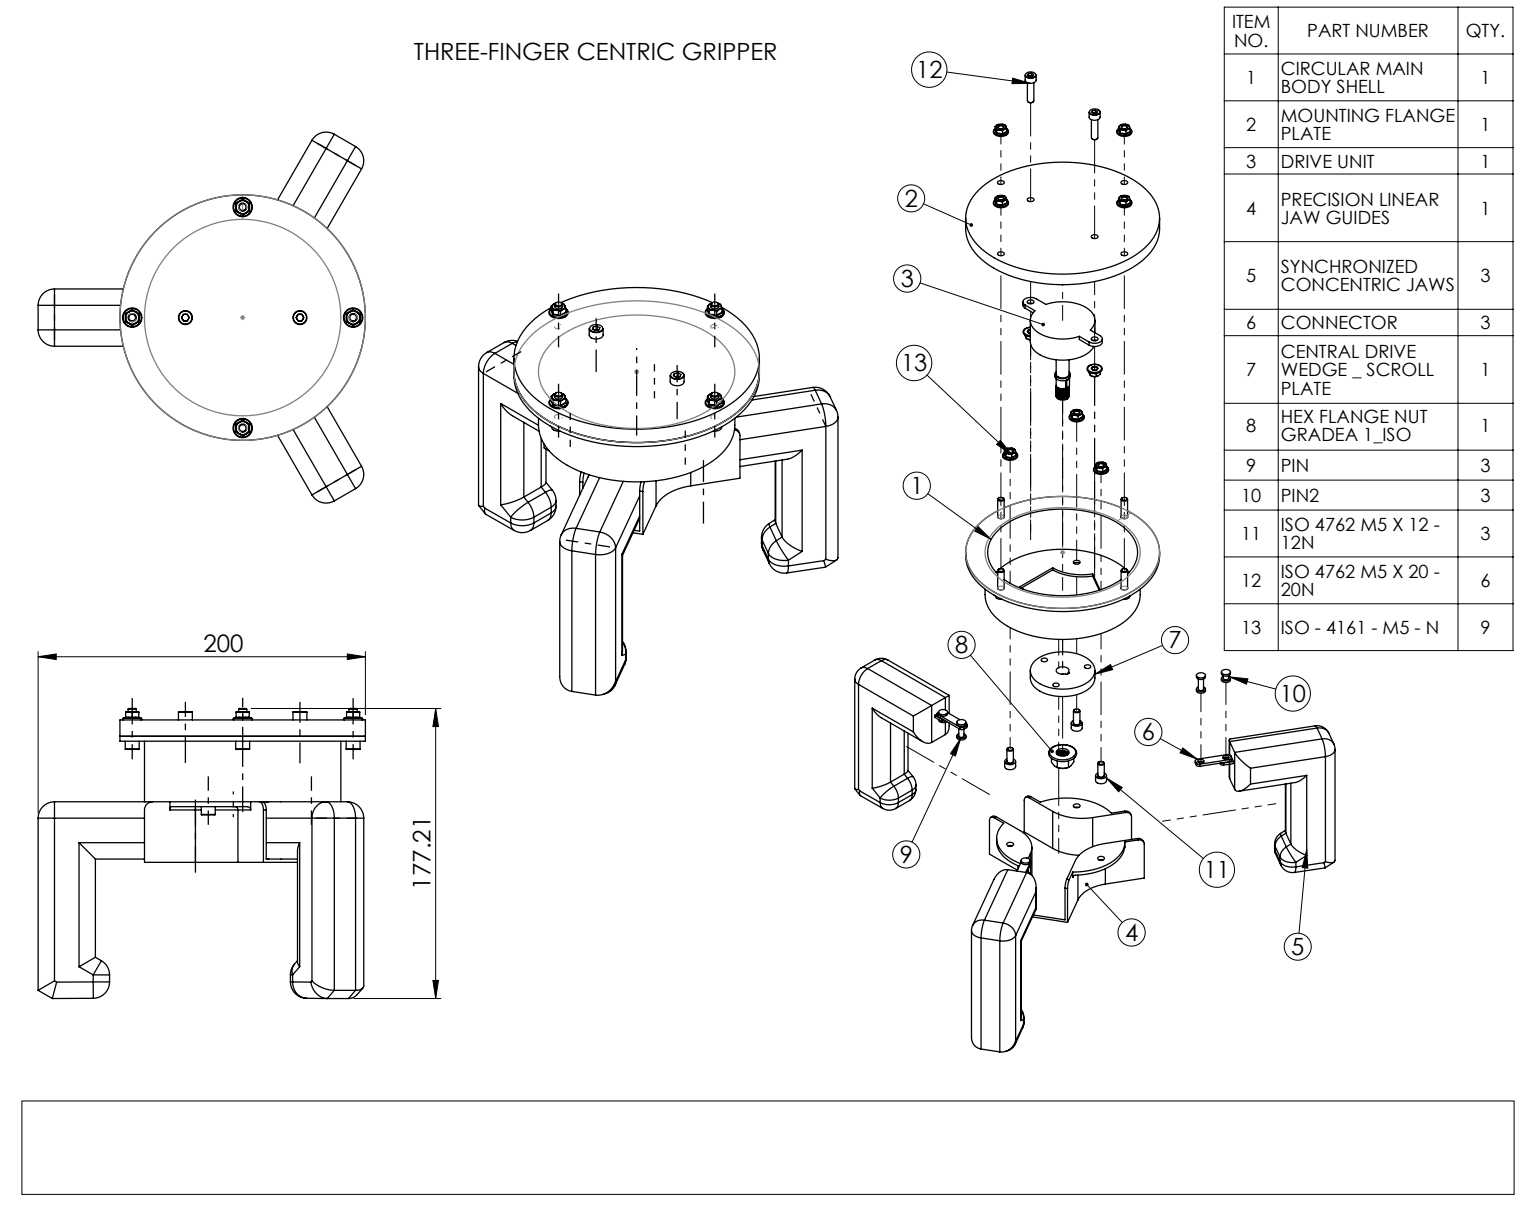
ISO-10303-21;
HEADER;
FILE_DESCRIPTION (('STEP AP214'),
    '1' );
FILE_NAME ('BR-003',
    '2026-10-08T13:56:24',
    ( '' ),
    ( '' ),
    'SwSTEP 2.0',
    'SolidWorks 2026',
    '' );
FILE_SCHEMA (( 'AUTOMOTIVE_DESIGN' ));
ENDSEC;

DATA;
#1 = ORIENTED_EDGE ( 'NONE', *, *, #6878, .F. ) ;
#2 = EDGE_CURVE ( 'NONE', #5376, #11920, #8952, .T. ) ;
#3 = CARTESIAN_POINT ( 'NONE',  ( -7.500000000000003553, -3.160302461882598557, -7.231849989190477501 ) ) ;
#4 = CARTESIAN_POINT ( 'NONE',  ( -1.846868145590737420, -24.75000000136559564, 4.458734124999999437 ) ) ;
#5 = FACE_OUTER_BOUND ( 'NONE', #2226, .T. ) ;
#6 = VERTEX_POINT ( 'NONE', #1075 ) ;
#7 = CARTESIAN_POINT ( 'NONE',  ( -19.99999999999956657, -20.00000000000000000, 2.500000000000877520 ) ) ;
#8 = CARTESIAN_POINT ( 'NONE',  ( 0.000000000000000000, 50.00000000000000000, -75.00000000000004263 ) ) ;
#9 = DIRECTION ( 'NONE',  ( -1.000000000000000000, -0.000000000000000000, -0.000000000000000000 ) ) ;
#10 = FACE_OUTER_BOUND ( 'NONE', #8516, .T. ) ;
#11 = CARTESIAN_POINT ( 'NONE',  ( 1.846868145590735200, -25.50000000136559919, -4.458734125000000326 ) ) ;
#12 = DIRECTION ( 'NONE',  ( 0.000000000000000000, 0.000000000000000000, 1.000000000000000000 ) ) ;
#13 =( REPRESENTATION_RELATIONSHIP ('NONE','NONE', #4176, #790 ) REPRESENTATION_RELATIONSHIP_WITH_TRANSFORMATION ( #11413 )SHAPE_REPRESENTATION_RELATIONSHIP( ) );
#14 = CARTESIAN_POINT ( 'NONE',  ( 19.99999999999956657, -8.786575603324269439E-13, 0.000000000000000000 ) ) ;
#15 = CARTESIAN_POINT ( 'NONE',  ( -3.535533905932738641, -28.50000000273118772, 3.535533905932737309 ) ) ;
#16 = CARTESIAN_POINT ( 'NONE',  ( 7.922281120364393914, 4.573931137438269623, -8.047472243342932430 ) ) ;
#17 = CARTESIAN_POINT ( 'NONE',  ( 3.152801135295367541, -29.31250000136559208, -3.152801135295367541 ) ) ;
#18 = ADVANCED_FACE ( 'NONE', ( #40 ), #4954, .F. ) ;
#19 = CYLINDRICAL_SURFACE ( 'NONE', #13536, 2.649999999999992806 ) ;
#21 = ADVANCED_FACE ( 'NONE', ( #13423 ), #15876, .F. ) ;
#20 = ORIENTED_EDGE ( 'NONE', *, *, #13802, .F. ) ;
#22 = EDGE_CURVE ( 'NONE', #14589, #7997, #9723, .T. ) ;
#23 = SURFACE_STYLE_FILL_AREA ( #9793 ) ;
#24 = ORIENTED_EDGE ( 'NONE', *, *, #9310, .F. ) ;
#25 = DIRECTION ( 'NONE',  ( -0.000000000000000000, -1.000000000000000000, -0.000000000000000000 ) ) ;
#26 = ORIENTED_EDGE ( 'NONE', *, *, #11739, .T. ) ;
#27 = FACE_BOUND ( 'NONE', #8966, .T. ) ;
#28 = CARTESIAN_POINT ( 'NONE',  ( 2.500000000000000000, -1.768423874527823569, 1.021000000000002794 ) ) ;
#29 = CARTESIAN_POINT ( 'NONE',  ( -3.033343224707664376, 3.753672977998667726, -2.999999998634409248 ) ) ;
#30 = APPLICATION_PROTOCOL_DEFINITION ( 'draft international standard', 'automotive_design', 1998, #15187 ) ;
#31 = CARTESIAN_POINT ( 'NONE',  ( 0.5093500532425063732, 4.799145180956616130, -5.374999998634406140 ) ) ;
#32 = SURFACE_STYLE_USAGE ( .BOTH. , #3487 ) ;
#33 = DIRECTION ( 'NONE',  ( 0.000000000000000000, 1.000000000000000000, 0.000000000000000000 ) ) ;
#34 =( BOUNDED_CURVE ( )  B_SPLINE_CURVE ( 2, ( #15482, #12870, #10698, #767, #4553, #15316, #15635, #9486, #1883, #6824, #14418 ),
 .UNSPECIFIED., .F., .F. ) 
 B_SPLINE_CURVE_WITH_KNOTS ( ( 3, 2, 2, 2, 2, 3 ),
 ( 0.2545872658012772738, 0.2625000000000000111, 0.2750000000000000222, 0.2874999999999999778, 0.2999999999999999889, 0.3045872658012772627 ),
 .UNSPECIFIED. ) 
 CURVE ( )  GEOMETRIC_REPRESENTATION_ITEM ( )  RATIONAL_B_SPLINE_CURVE ( ( 0.9646335149384808183, 0.9518143178943437865, 1.000000000000000000, 0.9238795325112867385, 1.000000000000000000, 0.9238795325112867385, 1.000000000000000000, 0.9238795325112867385, 1.000000000000000000, 0.9720652146169430630, 0.9646335149384808183 ) ) 
 REPRESENTATION_ITEM ( '' )  );
#35 = LINE ( 'NONE', #1227, #14934 ) ;
#36 = EDGE_CURVE ( 'NONE', #5349, #13611, #14887, .T. ) ;
#37 =( NAMED_UNIT ( * ) PLANE_ANGLE_UNIT ( ) SI_UNIT ( $, .RADIAN. ) );
#38 = ORIENTED_EDGE ( 'NONE', *, *, #402, .T. ) ;
#39 = CARTESIAN_POINT ( 'NONE',  ( 4.197310751797292738, 0.8178363989516252985, -3.502498386812444409 ) ) ;
#40 = FACE_OUTER_BOUND ( 'NONE', #10361, .T. ) ;
#41 = ORIENTED_EDGE ( 'NONE', *, *, #9292, .F. ) ;
#42 = CARTESIAN_POINT ( 'NONE',  ( -1.261996585732579224, 4.276409079477648589, -4.312499998634405252 ) ) ;
#43 = PRODUCT_DEFINITION_SHAPE ( 'NONE', 'NONE',  #15984 ) ;
#44 = CARTESIAN_POINT ( 'NONE',  ( 45.58845726811988897, -5.000000000000004441, 42.96152422706634155 ) ) ;
#45 = LINE ( 'NONE', #8777, #8712 ) ;
#46 = CARTESIAN_POINT ( 'NONE',  ( -5.000000000000091482, -0.7223674278660691117, -2.521799365517155334 ) ) ;
#47 = FACE_OUTER_BOUND ( 'NONE', #13583, .T. ) ;
#48 = CARTESIAN_POINT ( 'NONE',  ( 3.401574460001763001, -4.209348295687703967, 0.9375000027311842787 ) ) ;
#49 = CARTESIAN_POINT ( 'NONE',  ( -2.071067811865478170, -24.31250000000000000, 5.000000000000000000 ) ) ;
#50 = CARTESIAN_POINT ( 'NONE',  ( 5.000000000000000000, -28.18750000273119127, 2.071067811865478614 ) ) ;
#51 = CARTESIAN_POINT ( 'NONE',  ( -4.458734124999999437, -26.25000000136559564, -1.846868145590735644 ) ) ;
#52 = CARTESIAN_POINT ( 'NONE',  ( 3.152801135295366208, -23.56250000136559564, 3.152801135295367985 ) ) ;
#53 = CARTESIAN_POINT ( 'NONE',  ( -3.753672977998669946, -3.033343224707661712, -4.749999998634407028 ) ) ;
#54 = LINE ( 'NONE', #13437, #11247 ) ;
#55 = ORIENTED_EDGE ( 'NONE', *, *, #1011, .T. ) ;
#56 = ORIENTED_EDGE ( 'NONE', *, *, #13519, .T. ) ;
#57 = AXIS2_PLACEMENT_3D ( 'NONE', #12926, #4133, #15222 ) ;
#58 = CARTESIAN_POINT ( 'NONE',  ( 0.000000000000000000, 0.000000000000000000, 0.000000000000000000 ) ) ;
#59 = VERTEX_POINT ( 'NONE', #6499 ) ;
#60 = CARTESIAN_POINT ( 'NONE',  ( -4.458734124999999437, -23.18750000136559564, -5.460374474430324690E-16 ) ) ;
#61 = CARTESIAN_POINT ( 'NONE',  ( 2.500000000000000000, 2.500728763858895382E-16, -2.041999999999999815 ) ) ;
#62 = CARTESIAN_POINT ( 'NONE',  ( -9.184850993605147944E-16, -30.37500000273118772, 5.000000000000000888 ) ) ;
#63 = EDGE_CURVE ( 'NONE', #10036, #14429, #10056, .T. ) ;
#64 = DIRECTION ( 'NONE',  ( 0.000000000000000000, 0.000000000000000000, 1.000000000000000000 ) ) ;
#65 = CARTESIAN_POINT ( 'NONE',  ( 4.896370289181515290, -5.000000000000000000, 48.48076211353313170 ) ) ;
#66 = CARTESIAN_POINT ( 'NONE',  ( -5.000000000000003553, -1.404940523648820476E-14, -7.545263047592946748 ) ) ;
#67 = CARTESIAN_POINT ( 'NONE',  ( 4.391654775818395251, -2.390265326283149694, -0.1250000000000035805 ) ) ;
#68 = CARTESIAN_POINT ( 'NONE',  ( -4.209348295687703079, -3.401574460001763445, -2.312499997268814944 ) ) ;
#69 = CARTESIAN_POINT ( 'NONE',  ( -3.535533905932737309, -27.62500000000000000, -3.535533905932738197 ) ) ;
#70 = CARTESIAN_POINT ( 'NONE',  ( 1.846868145590736310, -28.62500000136559919, 4.458734124999999437 ) ) ;
#71 = CARTESIAN_POINT ( 'NONE',  ( -3.033343224707664376, 3.753672977998667726, -2.249999998634408804 ) ) ;
#72 = ORIENTED_EDGE ( 'NONE', *, *, #13780, .T. ) ;
#73 = FACE_OUTER_BOUND ( 'NONE', #11557, .T. ) ;
#74 = VERTEX_POINT ( 'NONE', #3974 ) ;
#75 = ORIENTED_EDGE ( 'NONE', *, *, #13958, .T. ) ;
#76 = DIRECTION ( 'NONE',  ( 0.000000000000000000, 1.000000000000000000, 0.000000000000000000 ) ) ;
#77 = CARTESIAN_POINT ( 'NONE',  ( 2.730187237215162345E-16, -26.18750000136559564, -4.458734124999999437 ) ) ;
#78 = DIRECTION ( 'NONE',  ( -1.000000000000000000, 0.000000000000000000, 0.000000000000000000 ) ) ;
#79 = VERTEX_POINT ( 'NONE', #13671 ) ;
#80 = LINE ( 'NONE', #11141, #9950 ) ;
#81 = VECTOR ( 'NONE', #2135, 1000.000000000000000 ) ;
#82 = CYLINDRICAL_SURFACE ( 'NONE', #8761, 60.00000000000000000 ) ;
#83 = EDGE_CURVE ( 'NONE', #1457, #7914, #2680, .T. ) ;
#84 = FACE_OUTER_BOUND ( 'NONE', #4287, .T. ) ;
#85 = PLANE ( 'NONE',  #15054 ) ;
#86 = EDGE_CURVE ( 'NONE', #59, #10154, #4028, .T. ) ;
#87 = CARTESIAN_POINT ( 'NONE',  ( -3.535533905932738641, -30.37500000000000000, 3.535533905932737309 ) ) ;
#88 = CARTESIAN_POINT ( 'NONE',  ( 16.55500000000001393, 0.000000000000000000, 2.500000000000000444 ) ) ;
#89 = DIRECTION ( 'NONE',  ( 0.000000000000000000, 0.000000000000000000, 1.000000000000000000 ) ) ;
#90 = CARTESIAN_POINT ( 'NONE',  ( 3.535533905932738197, -27.00000000273118772, -3.535533905932738197 ) ) ;
#91 = DIRECTION ( 'NONE',  ( -1.000000000000000000, -0.000000000000000000, -0.000000000000000000 ) ) ;
#92 = PLANE ( 'NONE',  #4586 ) ;
#93 = ORIENTED_EDGE ( 'NONE', *, *, #6840, .T. ) ;
#94 = PRESENTATION_STYLE_ASSIGNMENT (( #15940 ) ) ;
#95 = ORIENTED_EDGE ( 'NONE', *, *, #15170, .F. ) ;
#96 = CARTESIAN_POINT ( 'NONE',  ( -1.655952806101422814, 3.662737355149034979, -7.623296525288699970E-18 ) ) ;
#97 = ORIENTED_EDGE ( 'NONE', *, *, #4296, .T. ) ;
#98 = DIRECTION ( 'NONE',  ( -1.000000000000000000, -0.000000000000000000, -0.000000000000000000 ) ) ;
#99 = APPLICATION_CONTEXT ( 'automotive_design' ) ;
#100 = EDGE_CURVE ( 'NONE', #1601, #9532, #5846, .T. ) ;
#101 = VECTOR ( 'NONE', #11182, 1000.000000000000000 ) ;
#102 = EDGE_CURVE ( 'NONE', #3403, #4061, #7930, .T. ) ;
#103 = CARTESIAN_POINT ( 'NONE',  ( 40.98096197216263903, -3.000000000000000000, 26.98110827883376928 ) ) ;
#104 = CARTESIAN_POINT ( 'NONE',  ( 0.5093500532425063732, 4.799145180956616130, -2.124999998634406584 ) ) ;
#105 = APPLICATION_PROTOCOL_DEFINITION ( 'draft international standard', 'automotive_design', 1998, #14975 ) ;
#106 = CARTESIAN_POINT ( 'NONE',  ( -3.916244202832140253, 2.131511515620587272, -5.187499998634406140 ) ) ;
#107 = CARTESIAN_POINT ( 'NONE',  ( 5.000000000000004441, 5.204748896376250699E-16, -4.250000000000000000 ) ) ;
#108 = CARTESIAN_POINT ( 'NONE',  ( 5.000000000000000000, -24.06250000000000000, 2.071067811865478614 ) ) ;
#109 = ORIENTED_EDGE ( 'NONE', *, *, #12160, .T. ) ;
#110 = LINE ( 'NONE', #12615, #13102 ) ;
#111 = ORIENTED_EDGE ( 'NONE', *, *, #9988, .F. ) ;
#112 = DIRECTION ( 'NONE',  ( -1.925929944387236904E-30, 1.000000000000000000, -1.387778780781445676E-15 ) ) ;
#113 = FACE_OUTER_BOUND ( 'NONE', #15026, .T. ) ;
#114 = STYLED_ITEM ( 'NONE', ( #1544 ), #1156 ) ;
#115 = ORIENTED_EDGE ( 'NONE', *, *, #5097, .T. ) ;
#116 = ITEM_DEFINED_TRANSFORMATION ( 'NONE', 'NONE', #11467,  #3223 ) ;
#117 = CARTESIAN_POINT ( 'NONE',  ( -4.799145180956616130, 0.5093500532425063732, -2.124999998634406584 ) ) ;
#118 = DIRECTION ( 'NONE',  ( 0.000000000000000000, 0.000000000000000000, -1.000000000000000000 ) ) ;
#119 = EDGE_CURVE ( 'NONE', #13173, #1506, #10244, .T. ) ;
#120 = EDGE_CURVE ( 'NONE', #12835, #7197, #1963, .T. ) ;
#121 = DIRECTION ( 'NONE',  ( 0.000000000000000000, -1.000000000000000000, 0.000000000000000000 ) ) ;
#122 = DIRECTION ( 'NONE',  ( 0.000000000000000000, 0.000000000000000000, -1.000000000000000000 ) ) ;
#123 = UNCERTAINTY_MEASURE_WITH_UNIT (LENGTH_MEASURE( 1.000000000000000082E-05 ), #6249, 'distance_accuracy_value', 'NONE');
#124 = CARTESIAN_POINT ( 'NONE',  ( -9.184850993605147944E-16, -27.37500000273118772, 5.000000000000000000 ) ) ;
#125 = AXIS2_PLACEMENT_3D ( 'NONE', #6082, #4708, #13105 ) ;
#126 = CARTESIAN_POINT ( 'NONE',  ( -5.381735091635034607, 0.5711823568785950878, -3.437499997268817609 ) ) ;
#127 = DIRECTION ( 'NONE',  ( -1.000000000000000000, -0.000000000000000000, -0.000000000000000000 ) ) ;
#128 = FACE_OUTER_BOUND ( 'NONE', #6380, .T. ) ;
#129 = CARTESIAN_POINT ( 'NONE',  ( 3.152801135295366208, -23.81250000136559564, 3.152801135295367985 ) ) ;
#130 = ORIENTED_EDGE ( 'NONE', *, *, #2112, .F. ) ;
#131 = AXIS2_PLACEMENT_3D ( 'NONE', #700, #8225, #6765 ) ;
#132 = DIRECTION ( 'NONE',  ( -0.000000000000000000, -1.000000000000000000, -0.000000000000000000 ) ) ;
#133 = CARTESIAN_POINT ( 'NONE',  ( -1.261996585732579224, 4.276409079477648589, -5.062499998634406140 ) ) ;
#134 = DIRECTION ( 'NONE',  ( 1.000000000000000000, 0.000000000000000000, 0.000000000000000000 ) ) ;
#135 = EDGE_LOOP ( 'NONE', ( #5012, #11685, #4576, #2768 ) ) ;
#136 = EDGE_LOOP ( 'NONE', ( #1331, #8498 ) ) ;
#137 = PRESENTATION_STYLE_ASSIGNMENT (( #9992 ) ) ;
#138 = VERTEX_POINT ( 'NONE', #361 ) ;
#139 = CARTESIAN_POINT ( 'NONE',  ( -1.846868145590737420, -25.00000000136559564, 4.458734124999999437 ) ) ;
#140 = DIRECTION ( 'NONE',  ( 0.000000000000000000, 0.000000000000000000, -1.000000000000000000 ) ) ;
#141 = STYLED_ITEM ( 'NONE', ( #7237 ), #10261 ) ;
#142 = AXIS2_PLACEMENT_3D ( 'NONE', #6437, #6586, #9027 ) ;
#143 = PLANE ( 'NONE',  #15618 ) ;
#144 =( GEOMETRIC_REPRESENTATION_CONTEXT ( 3 ) GLOBAL_UNCERTAINTY_ASSIGNED_CONTEXT ( ( #8076 ) ) GLOBAL_UNIT_ASSIGNED_CONTEXT ( ( #8304, #5944, #13354 ) ) REPRESENTATION_CONTEXT ( 'NONE', 'WORKASPACE' ) );
#145 = EDGE_CURVE ( 'NONE', #14420, #4422, #3824, .T. ) ;
#146 = CARTESIAN_POINT ( 'NONE',  ( -1.306442393143577574, -8.377108146505392483, -7.792327460285857654 ) ) ;
#147 = CARTESIAN_POINT ( 'NONE',  ( -2.500000000000011102, 7.216878364870347617, -7.063244554130012176 ) ) ;
#148 = CARTESIAN_POINT ( 'NONE',  ( -31.74999999999995737, 0.000000000000000000, 4.250000000000000000 ) ) ;
#149 = CARTESIAN_POINT ( 'NONE',  ( 4.391654775818395251, -2.390265326283149694, -5.125000000000000888 ) ) ;
#150 = LINE ( 'NONE', #12166, #14801 ) ;
#151 = DIRECTION ( 'NONE',  ( 0.000000000000000000, 1.000000000000000000, 0.000000000000000000 ) ) ;
#152 = CARTESIAN_POINT ( 'NONE',  ( -1.846868145590734756, -25.12500000136559564, -4.458734125000000326 ) ) ;
#153 = CARTESIAN_POINT ( 'NONE',  ( -3.033343224707664376, 3.753672977998667726, -1.249999998634407916 ) ) ;
#154 = ORIENTED_EDGE ( 'NONE', *, *, #781, .T. ) ;
#155 = AXIS2_PLACEMENT_3D ( 'NONE', #3936, #13786, #7593 ) ;
#156 = DIRECTION ( 'NONE',  ( 0.000000000000000000, 1.000000000000000000, -0.000000000000000000 ) ) ;
#157 = B_SPLINE_CURVE_WITH_KNOTS ( 'NONE', 3,
 ( #8766, #7551, #13667, #2597, #1388, #6333, #11408, #199, #5118 ),
 .UNSPECIFIED., .F., .F.,
 ( 4, 2, 1, 2, 4 ),
 ( 0.000000000000000000, 0.002165063509461097498, 0.004330127018922194995, 0.006495190528383292493, 0.008660254037844389990 ),
 .UNSPECIFIED. ) ;
#158 = ORIENTED_EDGE ( 'NONE', *, *, #11026, .F. ) ;
#159 = ORIENTED_EDGE ( 'NONE', *, *, #7096, .F. ) ;
#161 = CARTESIAN_POINT ( 'NONE',  ( 11.91154273188013768, 0.000000000000000000, -56.63139720814412925 ) ) ;
#160 = VECTOR ( 'NONE', #2348, 1000.000000000000000 ) ;
#162 = AXIS2_PLACEMENT_3D ( 'NONE', #1282, #2402, #6227 ) ;
#163 = CARTESIAN_POINT ( 'NONE',  ( -4.458734124999999437, -25.93750000136559564, -5.460374474430324690E-16 ) ) ;
#164 = ADVANCED_FACE ( 'NONE', ( #12534 ), #7474, .T. ) ;
#165 = CARTESIAN_POINT ( 'NONE',  ( 0.000000000000000000, -13.00000000000000178, 0.000000000000000000 ) ) ;
#166 = EDGE_LOOP ( 'NONE', ( #524, #8301 ) ) ;
#167 = VECTOR ( 'NONE', #2072, 1000.000000000000000 ) ;
#168 = CARTESIAN_POINT ( 'NONE',  ( 6.123233995736766282E-16, -20.00000000000000000, -5.000000000000000000 ) ) ;
#169 = CARTESIAN_POINT ( 'NONE',  ( 3.753672977998667726, 3.033343224707664820, -3.249999998634409692 ) ) ;
#170 = CARTESIAN_POINT ( 'NONE',  ( -19.99999999999956657, -13.00000000000000178, -2.499999999999120259 ) ) ;
#171 = VECTOR ( 'NONE', #2459, 1000.000000000000114 ) ;
#172 = CARTESIAN_POINT ( 'NONE',  ( 3.061616997868383141E-16, -30.75000000000000000, -5.000000000000000000 ) ) ;
#173 = CARTESIAN_POINT ( 'NONE',  ( -0.02511973781850462134, 4.877415612947412882, -3.751298745799839462 ) ) ;
#174 = PLANE ( 'NONE',  #5147 ) ;
#175 = CARTESIAN_POINT ( 'NONE',  ( -3.535533905932738641, -27.50000000273118772, 3.535533905932737309 ) ) ;
#176 = CARTESIAN_POINT ( 'NONE',  ( 3.280815508853480278, 7.221948645665444921, -7.591546097228401457 ) ) ;
#177 = CARTESIAN_POINT ( 'NONE',  ( -1.846868145590734756, -31.12500000136559564, -4.458734124999999437 ) ) ;
#178 = PRESENTATION_STYLE_ASSIGNMENT (( #1292 ) ) ;
#179 = ORIENTED_EDGE ( 'NONE', *, *, #11221, .F. ) ;
#180 = CIRCLE ( 'NONE', #13308, 2.649999999999985700 ) ;
#181 = ORIENTED_EDGE ( 'NONE', *, *, #2624, .T. ) ;
#182 = SHAPE_REPRESENTATION_RELATIONSHIP ( 'NONE' , 'NONE' ,  #1906, #2911 ) ;
#184 = ORIENTED_EDGE ( 'NONE', *, *, #8002, .F. ) ;
#183 = EDGE_CURVE ( 'NONE', #10747, #715, #1391, .T. ) ;
#185 = DIRECTION ( 'NONE',  ( 1.000000000000000000, 0.000000000000000000, 0.000000000000000000 ) ) ;
#186 = EDGE_CURVE ( 'NONE', #6462, #4993, #11776, .T. ) ;
#187 = AXIS2_PLACEMENT_3D ( 'NONE', #15569, #9111, #5544 ) ;
#188 = EDGE_LOOP ( 'NONE', ( #9536, #20, #1499, #15874 ) ) ;
#189 = CLOSED_SHELL ( 'NONE', ( #8416, #4530, #5345, #11458, #1142, #6838, #2428, #15032, #9127, #8023, #1756, #11349, #15010, #2861, #6382, #12271, #10045, #7422, #518, #1324, #8465, #1380, #7833, #9352, #14029, #11070, #15391 ) ) ;
#190 = VECTOR ( 'NONE', #3523, 1000.000000000000000 ) ;
#191 = CARTESIAN_POINT ( 'NONE',  ( 39.53738644055469820, -5.000000000000000000, -28.48076211352550047 ) ) ;
#192 = CARTESIAN_POINT ( 'NONE',  ( 2.131511515620586383, 3.916244202832140253, -3.187499998634407916 ) ) ;
#193 = CARTESIAN_POINT ( 'NONE',  ( -4.000000000000000000, -2.309401076758512694, -5.000000000000000000 ) ) ;
#194 = CIRCLE ( 'NONE', #13575, 2.500000000000000444 ) ;
#195 = CARTESIAN_POINT ( 'NONE',  ( 4.799145180956616130, -0.5093500532425063732, -6.624999998634407916 ) ) ;
#196 = DIRECTION ( 'NONE',  ( 0.000000000000000000, 1.000000000000000000, 0.000000000000000000 ) ) ;
#197 = DIRECTION ( 'NONE',  ( -0.9591083387322728582, -0.2830392103123166025, 0.000000000000000000 ) ) ;
#198 = ORIENTED_EDGE ( 'NONE', *, *, #1877, .T. ) ;
#199 = CARTESIAN_POINT ( 'NONE',  ( -7.500000000000000888, -3.608439182435168036, -7.298562697733108173 ) ) ;
#200 =( NAMED_UNIT ( * ) SI_UNIT ( $, .STERADIAN. ) SOLID_ANGLE_UNIT ( ) );
#201 = ORIENTED_EDGE ( 'NONE', *, *, #2412, .F. ) ;
#202 = FACE_OUTER_BOUND ( 'NONE', #2206, .T. ) ;
#203 = CIRCLE ( 'NONE', #1999, 2.649999999999992806 ) ;
#204 = CARTESIAN_POINT ( 'NONE',  ( 1.846868145590735200, -31.25000000136559564, -4.458734125000000326 ) ) ;
#205 = EDGE_CURVE ( 'NONE', #14772, #10685, #7688, .T. ) ;
#206 = ORIENTED_EDGE ( 'NONE', *, *, #3407, .T. ) ;
#207 = CONTEXT_DEPENDENT_SHAPE_REPRESENTATION ( #6089, #7942 ) ;
#208 = CARTESIAN_POINT ( 'NONE',  ( -4.799145180956616130, 0.5093500532425063732, -8.124999998634407916 ) ) ;
#209 = CARTESIAN_POINT ( 'NONE',  ( 4.000000000000000000, 0.3987449864460005378, -0.01220643443059817035 ) ) ;
#210 = CARTESIAN_POINT ( 'NONE',  ( -4.795541693661363958, -1.415196051561583790, -5.374999997268817609 ) ) ;
#211 = AXIS2_PLACEMENT_3D ( 'NONE', #9858, #13319, #2262 ) ;
#212 = CARTESIAN_POINT ( 'NONE',  ( -44.99999999999999289, -11.00000000000000178, 4.000000000000831335 ) ) ;
#213 = AXIS2_PLACEMENT_3D ( 'NONE', #6440, #11355, #304 ) ;
#214 = CARTESIAN_POINT ( 'NONE',  ( 4.211140560182196957, -2.431303136016555122, -3.745885042887436622 ) ) ;
#215 = CARTESIAN_POINT ( 'NONE',  ( -4.209348295687703967, -3.401574460001763001, -5.312499997268816720 ) ) ;
#216 = CARTESIAN_POINT ( 'NONE',  ( 3.061616997868383141E-16, -26.87500000273118772, -5.000000000000000000 ) ) ;
#217 = CARTESIAN_POINT ( 'NONE',  ( 3.061616997868383141E-16, -27.87500000273118772, -5.000000000000000000 ) ) ;
#218 = CARTESIAN_POINT ( 'NONE',  ( -1.846868145590737420, -22.00000000136559208, 4.458734124999997661 ) ) ;
#219 = EDGE_LOOP ( 'NONE', ( #418, #2815, #404, #4757, #14320 ) ) ;
#220 = DIRECTION ( 'NONE',  ( -1.000000000000000000, -0.000000000000000000, -0.000000000000000000 ) ) ;
#221 = DIRECTION ( 'NONE',  ( -1.000000000000000000, -0.000000000000000000, -0.000000000000000000 ) ) ;
#222 = DIRECTION ( 'NONE',  ( -0.000000000000000000, 1.000000000000000000, -0.000000000000000000 ) ) ;
#223 = EDGE_CURVE ( 'NONE', #8492, #2510, #15229, .T. ) ;
#224 = ORIENTED_EDGE ( 'NONE', *, *, #11721, .F. ) ;
#225 = EDGE_LOOP ( 'NONE', ( #5891, #2747, #6648, #4937, #7254 ) ) ;
#226 = EDGE_CURVE ( 'NONE', #3694, #59, #13994, .T. ) ;
#227 = EDGE_CURVE ( 'NONE', #9634, #14535, #13577, .T. ) ;
#228 = ADVANCED_FACE ( 'NONE', ( #113 ), #1674, .T. ) ;
#229 = ORIENTED_EDGE ( 'NONE', *, *, #1759, .F. ) ;
#230 = CARTESIAN_POINT ( 'NONE',  ( -4.336808689942017736E-16, 9.147862274876558786, -8.047472243342932430 ) ) ;
#231 = AXIS2_PLACEMENT_3D ( 'NONE', #4894, #14440, #11914 ) ;
#232 = CARTESIAN_POINT ( 'NONE',  ( 0.000000000000000000, 0.000000000000000000, 0.000000000000000000 ) ) ;
#233 = VECTOR ( 'NONE', #8677, 1000.000000000000114 ) ;
#234 = CARTESIAN_POINT ( 'NONE',  ( 4.458734124999999437, -31.56250000136559564, 0.000000000000000000 ) ) ;
#235 = VECTOR ( 'NONE', #12531, 1000.000000000000114 ) ;
#236 = DIRECTION ( 'NONE',  ( -0.8191520442889902442, 0.000000000000000000, -0.5735764363510482688 ) ) ;
#237 = CARTESIAN_POINT ( 'NONE',  ( 0.000000000000000000, 37.00000000000000000, 0.000000000000000000 ) ) ;
#238 = CARTESIAN_POINT ( 'NONE',  ( -115.0000000000000142, -3.122502256758252770E-14, 7.500000000000001776 ) ) ;
#239 = CARTESIAN_POINT ( 'NONE',  ( -4.391654775818395251, 2.390265326283148806, -5.625000000000001776 ) ) ;
#240 = CARTESIAN_POINT ( 'NONE',  ( 5.000000000000000000, -30.06250000000000000, 2.071067811865478614 ) ) ;
#241 = VECTOR ( 'NONE', #6289, 1000.000000000000000 ) ;
#242 = CARTESIAN_POINT ( 'NONE',  ( 2.500000000000000000, -1.768423874527823791, -1.020999999999998353 ) ) ;
#243 = CARTESIAN_POINT ( 'NONE',  ( -8.190561711645485556E-16, -26.68750000136559564, 4.458734124999999437 ) ) ;
#244 = CIRCLE ( 'NONE', #13904, 3.499999999999999556 ) ;
#245 = CARTESIAN_POINT ( 'NONE',  ( -4.276409079477644148, -1.261996585732578335, -7.062499998634407916 ) ) ;
#246 = ORIENTED_EDGE ( 'NONE', *, *, #2734, .T. ) ;
#247 = DIRECTION ( 'NONE',  ( 0.000000000000000000, 0.000000000000000000, -1.000000000000000000 ) ) ;
#248 = ORIENTED_EDGE ( 'NONE', *, *, #7361, .F. ) ;
#249 = ORIENTED_EDGE ( 'NONE', *, *, #671, .F. ) ;
#250 = EDGE_CURVE ( 'NONE', #4014, #15267, #13743, .T. ) ;
#251 = VECTOR ( 'NONE', #1802, 1000.000000000000000 ) ;
#252 = CARTESIAN_POINT ( 'NONE',  ( -4.458734125000001214, -23.87500000136559564, 1.846868145590734089 ) ) ;
#253 = CARTESIAN_POINT ( 'NONE',  ( -36.99999999999999289, -11.00000000000000178, 4.000000000000832223 ) ) ;
#254 = ORIENTED_EDGE ( 'NONE', *, *, #15050, .F. ) ;
#255 = FACE_OUTER_BOUND ( 'NONE', #7312, .T. ) ;
#256 = AXIS2_PLACEMENT_3D ( 'NONE', #544, #2863, #5079 ) ;
#257 = DIRECTION ( 'NONE',  ( -0.000000000000000000, 1.000000000000000000, -0.000000000000000000 ) ) ;
#258 = CARTESIAN_POINT ( 'NONE',  ( 1.261996585732578113, -4.276409079477644148, -0.5624999986344088043 ) ) ;
#259 = FACE_OUTER_BOUND ( 'NONE', #15924, .T. ) ;
#260 = CARTESIAN_POINT ( 'NONE',  ( 5.000000000000000000, -29.00000000000000000, 0.000000000000000000 ) ) ;
#261 = DIRECTION ( 'NONE',  ( -1.000000000000000000, 0.000000000000000000, 1.239088197126290570E-16 ) ) ;
#262 = FACE_OUTER_BOUND ( 'NONE', #12296, .T. ) ;
#263 = CARTESIAN_POINT ( 'NONE',  ( 2.071067811865476394, -27.31250000273118417, 5.000000000000000000 ) ) ;
#264 = CARTESIAN_POINT ( 'NONE',  ( -5.000000000000004441, -1.011557177027151181E-15, -3.545263047592942307 ) ) ;
#265 = CARTESIAN_POINT ( 'NONE',  ( -8.190561711645485556E-16, -28.68750000136559564, 4.458734124999999437 ) ) ;
#266 = CARTESIAN_POINT ( 'NONE',  ( 2.500000000000000000, 2.357898499370433054, -1.951563910473907981E-15 ) ) ;
#267 = ORIENTED_EDGE ( 'NONE', *, *, #8923, .F. ) ;
#268 = ORIENTED_EDGE ( 'NONE', *, *, #2450, .T. ) ;
#269 = CIRCLE ( 'NONE', #3097, 2.041999999999999815 ) ;
#270 = ORIENTED_EDGE ( 'NONE', *, *, #4846, .T. ) ;
#271 = CARTESIAN_POINT ( 'NONE',  ( 0.000000000000000000, 0.000000000000000000, 0.000000000000000000 ) ) ;
#272 = ORIENTED_EDGE ( 'NONE', *, *, #10199, .F. ) ;
#273 = CARTESIAN_POINT ( 'NONE',  ( 0.000000000000000000, 0.000000000000000000, 0.000000000000000000 ) ) ;
#274 = CARTESIAN_POINT ( 'NONE',  ( 4.458734125000000326, -30.62500000136559208, -1.846868145590734978 ) ) ;
#275 = EDGE_CURVE ( 'NONE', #7055, #3403, #5959, .T. ) ;
#276 = ADVANCED_FACE ( 'NONE', ( #4161 ), #12794, .F. ) ;
#277 = DIRECTION ( 'NONE',  ( 0.000000000000000000, 0.000000000000000000, 1.000000000000000000 ) ) ;
#278 =( BOUNDED_CURVE ( )  B_SPLINE_CURVE ( 2, ( #14307, #13082, #15370, #11632, #13162, #12840, #4291, #11788, #15531 ),
 .UNSPECIFIED., .F., .F. ) 
 B_SPLINE_CURVE_WITH_KNOTS ( ( 3, 2, 2, 2, 3 ),
 ( 0.1750000000000001554, 0.1875000000000000833, 0.2000000000000000111, 0.2124999999999999389, 0.2249999999999998668 ),
 .UNSPECIFIED. ) 
 CURVE ( )  GEOMETRIC_REPRESENTATION_ITEM ( )  RATIONAL_B_SPLINE_CURVE ( ( 0.9999999999999990008, 0.9238795325112877377, 1.000000000000000000, 0.9238795325112867385, 1.000000000000000000, 0.9238795325112867385, 1.000000000000000000, 0.9238795325112876267, 0.9999999999999991118 ) ) 
 REPRESENTATION_ITEM ( '' )  );
#279 = SHAPE_REPRESENTATION ( 'pin', ( #3223 ), #1392 ) ;
#280 = CARTESIAN_POINT ( 'NONE',  ( -3.033343224707664376, 3.753672977998667726, -7.249999998634409692 ) ) ;
#281 = CARTESIAN_POINT ( 'NONE',  ( 7.500000000000004441, -4.330127018922205195, -1.000000000000000888 ) ) ;
#282 = LINE ( 'NONE', #2509, #5643 ) ;
#283 = ORIENTED_EDGE ( 'NONE', *, *, #4424, .F. ) ;
#284 = CARTESIAN_POINT ( 'NONE',  ( -5.560781378645573980, 0.000000000000000000, -4.000000000000000000 ) ) ;
#285 = ORIENTED_EDGE ( 'NONE', *, *, #7627, .F. ) ;
#286 = DIRECTION ( 'NONE',  ( -0.000000000000000000, -1.000000000000000000, -0.000000000000000000 ) ) ;
#287 = CARTESIAN_POINT ( 'NONE',  ( -28.86751345948129455, -35.00000000000000000, 49.99999999999999289 ) ) ;
#288 = ORIENTED_EDGE ( 'NONE', *, *, #2102, .T. ) ;
#289 = CARTESIAN_POINT ( 'NONE',  ( 4.799145180956616130, -0.5093500532425063732, -6.624999998634407916 ) ) ;
#290 = CARTESIAN_POINT ( 'NONE',  ( 4.000000000000000000, 0.7924765000094659007, -0.05906175389889852662 ) ) ;
#291 = CARTESIAN_POINT ( 'NONE',  ( -9.184850993605147944E-16, -28.37500000273118772, 5.000000000000000000 ) ) ;
#292 = EDGE_CURVE ( 'NONE', #10237, #3154, #5220, .T. ) ;
#293 = CARTESIAN_POINT ( 'NONE',  ( -9.184850993605147944E-16, -21.37500000273118772, 5.000000000000000000 ) ) ;
#294 = EDGE_CURVE ( 'NONE', #14177, #3976, #9330, .T. ) ;
#295 = PRODUCT_DEFINITION_CONTEXT ( 'detailed design', #4442, 'design' ) ;
#296 = PRODUCT_RELATED_PRODUCT_CATEGORY ( 'part', '', ( #8502 ) ) ;
#297 = CARTESIAN_POINT ( 'NONE',  ( 8.673617379884035472E-16, 4.618802153517012954, 0.000000000000000000 ) ) ;
#298 = CARTESIAN_POINT ( 'NONE',  ( -1.415196051561583790, 4.795541693661363958, -5.624999997268814944 ) ) ;
#299 = CARTESIAN_POINT ( 'NONE',  ( 4.209348295687701302, 3.401574460001766109, -8.812499997268812280 ) ) ;
#300 = DIRECTION ( 'NONE',  ( 1.000000000000000000, 0.000000000000000000, 0.000000000000000000 ) ) ;
#301 = CYLINDRICAL_SURFACE ( 'NONE', #15098, 2.649999999999992806 ) ;
#302 = ORIENTED_EDGE ( 'NONE', *, *, #11651, .T. ) ;
#303 = CARTESIAN_POINT ( 'NONE',  ( 0.000000000000000000, 0.000000000000000000, 0.000000000000000000 ) ) ;
#304 = DIRECTION ( 'NONE',  ( 0.000000000000000000, 0.000000000000000000, 1.000000000000000000 ) ) ;
#305 = CARTESIAN_POINT ( 'NONE',  ( -24.26932219902320043, 37.00000000000000000, -5.999999999999984901 ) ) ;
#306 = ORIENTED_EDGE ( 'NONE', *, *, #14745, .F. ) ;
#307 = VERTEX_POINT ( 'NONE', #7662 ) ;
#308 = ORIENTED_EDGE ( 'NONE', *, *, #7729, .F. ) ;
#309 = CARTESIAN_POINT ( 'NONE',  ( -4.613983237546152694, 6.452243898629810737, -7.591546097228399681 ) ) ;
#310 = DIRECTION ( 'NONE',  ( -1.000000000000000000, -2.775557561562892929E-15, 0.000000000000000000 ) ) ;
#311 = DIRECTION ( 'NONE',  ( -0.000000000000000000, 1.000000000000000000, -0.000000000000000000 ) ) ;
#312 = EDGE_CURVE ( 'NONE', #2273, #15957, #6128, .T. ) ;
#313 = DIRECTION ( 'NONE',  ( 0.000000000000000000, 0.000000000000000000, 1.000000000000000000 ) ) ;
#314 = CARTESIAN_POINT ( 'NONE',  ( -5.174575781537456898, -5.672711317431625488, -7.030005583190793494 ) ) ;
#315 = PRODUCT_RELATED_PRODUCT_CATEGORY ( 'part', '', ( #873 ) ) ;
#316 = EDGE_CURVE ( 'NONE', #15429, #4240, #2588, .T. ) ;
#317 = FACE_OUTER_BOUND ( 'NONE', #13857, .T. ) ;
#318 = CARTESIAN_POINT ( 'NONE',  ( 4.391654775818395251, -2.390265326283149694, -7.125000000000002665 ) ) ;
#319 = CARTESIAN_POINT ( 'NONE',  ( -158.0560796608385488, -84.57531754730580076, 7.500000000000001776 ) ) ;
#320 = DIRECTION ( 'NONE',  ( 0.000000000000000000, 0.000000000000000000, 1.000000000000000000 ) ) ;
#321 = CARTESIAN_POINT ( 'NONE',  ( -3.152801135295367985, -22.81250000136559564, 3.152801135295367096 ) ) ;
#322 = CARTESIAN_POINT ( 'NONE',  ( 1.261996585732578113, -4.276409079477644148, -6.812499998634407028 ) ) ;
#323 = ORIENTED_EDGE ( 'NONE', *, *, #1343, .T. ) ;
#324 = DIRECTION ( 'NONE',  ( 0.000000000000000000, 1.000000000000000000, 0.000000000000000000 ) ) ;
#325 = ORIENTED_EDGE ( 'NONE', *, *, #13615, .F. ) ;
#326 = ORIENTED_EDGE ( 'NONE', *, *, #10294, .F. ) ;
#327 = APPLICATION_CONTEXT ( 'automotive_design' ) ;
#328 = CARTESIAN_POINT ( 'NONE',  ( 1.846868145590735200, -22.25000000136559564, -4.458734125000000326 ) ) ;
#329 = DIRECTION ( 'NONE',  ( 0.000000000000000000, 0.000000000000000000, 1.000000000000000000 ) ) ;
#330 = ORIENTED_EDGE ( 'NONE', *, *, #5825, .T. ) ;
#331 = CARTESIAN_POINT ( 'NONE',  ( -5.000000000000000888, -28.56250000000000000, -2.071067811865475949 ) ) ;
#332 = CARTESIAN_POINT ( 'NONE',  ( 0.000000000000000000, -1.178949249685213863, 2.042000000000002924 ) ) ;
#333 = CARTESIAN_POINT ( 'NONE',  ( 3.753672977998667726, 3.033343224707664820, -2.249999998634408804 ) ) ;
#334 = CARTESIAN_POINT ( 'NONE',  ( 4.267391354405730475, 1.319746117868581647, -0.3789984458506751586 ) ) ;
#335 = EDGE_CURVE ( 'NONE', #10196, #14496, #7821, .T. ) ;
#336 = CARTESIAN_POINT ( 'NONE',  ( -3.535533905932737309, -29.62500000000000355, -3.535533905932738197 ) ) ;
#337 = CARTESIAN_POINT ( 'NONE',  ( -2.682243648011671588, -3.070208061305317759, -0.04852650426602272971 ) ) ;
#338 = LINE ( 'NONE', #12747, #2295 ) ;
#339 = CARTESIAN_POINT ( 'NONE',  ( 3.535533905932736864, -23.25000000273118772, 3.535533905932738641 ) ) ;
#340 = DIRECTION ( 'NONE',  ( 1.000000000000000000, 0.000000000000000000, 0.000000000000000000 ) ) ;
#341 = CARTESIAN_POINT ( 'NONE',  ( -9.184850993605147944E-16, -24.37500000273118772, 5.000000000000000000 ) ) ;
#342 = FILL_AREA_STYLE ('',( #5011 ) ) ;
#343 = ORIENTED_EDGE ( 'NONE', *, *, #4233, .F. ) ;
#344 = ORIENTED_EDGE ( 'NONE', *, *, #14576, .T. ) ;
#345 = AXIS2_PLACEMENT_3D ( 'NONE', #12427, #14786, #2573 ) ;
#346 = ORIENTED_EDGE ( 'NONE', *, *, #4980, .T. ) ;
#347 = AXIS2_PLACEMENT_3D ( 'NONE', #11601, #15335, #628 ) ;
#348 = CARTESIAN_POINT ( 'NONE',  ( 4.000000000000003553, -2.309401076758513138, -3.504271511726786859 ) ) ;
#349 = VERTEX_POINT ( 'NONE', #8867 ) ;
#350 = CARTESIAN_POINT ( 'NONE',  ( -90.00000000000000000, -95.00000000000000000, 7.500000000000001776 ) ) ;
#351 = CARTESIAN_POINT ( 'NONE',  ( -5.000000000000000000, -31.50000000000000000, -6.123233995736766282E-16 ) ) ;
#352 = PLANE ( 'NONE',  #15206 ) ;
#353 = VECTOR ( 'NONE', #2265, 1000.000000000000000 ) ;
#354 = CYLINDRICAL_SURFACE ( 'NONE', #57, 2.500000000000000444 ) ;
#355 = CARTESIAN_POINT ( 'NONE',  ( 1.261996585732578113, -4.276409079477644148, -3.812499998634408360 ) ) ;
#356 = DIRECTION ( 'NONE',  ( 0.000000000000000000, 0.000000000000000000, 1.000000000000000000 ) ) ;
#357 = ORIENTED_EDGE ( 'NONE', *, *, #14558, .T. ) ;
#358 = CARTESIAN_POINT ( 'NONE',  ( -19.99999999999956657, -20.00000000000000000, 8.786575603324269439E-13 ) ) ;
#359 = ORIENTED_EDGE ( 'NONE', *, *, #11812, .F. ) ;
#360 = CARTESIAN_POINT ( 'NONE',  ( 2.100000000000000089, 0.000000000000000000, -4.694516984716113228 ) ) ;
#361 = CARTESIAN_POINT ( 'NONE',  ( 67.49999999999931788, 40.00000000000000000, 2.650000000000013678 ) ) ;
#362 = VERTEX_POINT ( 'NONE', #11512 ) ;
#363 = CARTESIAN_POINT ( 'NONE',  ( 4.276409079477644148, 1.261996585732577891, -7.562499998634407916 ) ) ;
#364 = ADVANCED_FACE ( 'NONE', ( #4243 ), #462, .T. ) ;
#365 = CARTESIAN_POINT ( 'NONE',  ( 3.061616997868383043E-15, 20.00000000000000000, -25.00000000000000000 ) ) ;
#366 =( BOUNDED_CURVE ( )  B_SPLINE_CURVE ( 2, ( #11943, #1934, #7944, #15606, #11870, #816, #6883, #8181, #4525, #6731, #5816 ),
 .UNSPECIFIED., .F., .F. ) 
 B_SPLINE_CURVE_WITH_KNOTS ( ( 3, 2, 2, 2, 2, 3 ),
 ( 0.8045872658012773737, 0.8125000000000000000, 0.8249999999999999556, 0.8375000000000000222, 0.8499999999999999778, 0.8545872658012773071 ),
 .UNSPECIFIED. ) 
 CURVE ( )  GEOMETRIC_REPRESENTATION_ITEM ( )  RATIONAL_B_SPLINE_CURVE ( ( 0.9646335149384803742, 0.9518143178943441196, 1.000000000000000000, 0.9238795325112867385, 1.000000000000000000, 0.9238795325112867385, 1.000000000000000000, 0.9238795325112867385, 1.000000000000000000, 0.9720652146169428409, 0.9646335149384808183 ) ) 
 REPRESENTATION_ITEM ( '' )  );
#367 = CARTESIAN_POINT ( 'NONE',  ( 6.123233995736766282E-16, -20.00000000000000000, -5.000000000000000000 ) ) ;
#368 = CARTESIAN_POINT ( 'NONE',  ( 0.000000000000000000, 40.00000000000000000, 0.000000000000000000 ) ) ;
#369 = CARTESIAN_POINT ( 'NONE',  ( 4.391654775818395251, -2.390265326283149694, -2.999999997268815832 ) ) ;
#370 = DIRECTION ( 'NONE',  ( -1.000000000000000000, 0.000000000000000000, -0.000000000000000000 ) ) ;
#371 = CARTESIAN_POINT ( 'NONE',  ( -3.519724167363775358, 2.954775574544003636, -0.2910937876543309155 ) ) ;
#372 = CARTESIAN_POINT ( 'NONE',  ( 1.846868145590736310, -21.87500000136559208, 4.458734124999997661 ) ) ;
#373 = ORIENTED_EDGE ( 'NONE', *, *, #7059, .F. ) ;
#374 = DIRECTION ( 'NONE',  ( 0.000000000000000000, 0.000000000000000000, 1.000000000000000000 ) ) ;
#375 = CARTESIAN_POINT ( 'NONE',  ( 7.500000000000000888, 1.443375672974059665, -7.063244554130003294 ) ) ;
#376 = CARTESIAN_POINT ( 'NONE',  ( -3.535533905932738641, -26.50000000273118772, 3.535533905932737309 ) ) ;
#377 = ORIENTED_EDGE ( 'NONE', *, *, #15710, .F. ) ;
#378 = ORIENTED_EDGE ( 'NONE', *, *, #14411, .F. ) ;
#379 = VERTEX_POINT ( 'NONE', #1738 ) ;
#380 = CARTESIAN_POINT ( 'NONE',  ( -4.209348295687703079, -3.401574460001763445, -0.4375000000000013323 ) ) ;
#381 = ADVANCED_FACE ( 'NONE', ( #13861 ), #3996, .T. ) ;
#382 = DIRECTION ( 'NONE',  ( -0.000000000000000000, -1.000000000000000000, -0.000000000000000000 ) ) ;
#383 = EDGE_CURVE ( 'NONE', #5937, #2401, #5386, .T. ) ;
#384 = DIRECTION ( 'NONE',  ( -0.000000000000000000, 1.000000000000000000, -0.000000000000000000 ) ) ;
#385 = AXIS2_PLACEMENT_3D ( 'NONE', #8291, #2045, #4632 ) ;
#386 = CARTESIAN_POINT ( 'NONE',  ( 5.000000000000000000, 0.000000000000000000, 0.000000000000000000 ) ) ;
#387 = CIRCLE ( 'NONE', #3230, 2.649999999999985700 ) ;
#388 = PLANE ( 'NONE',  #14679 ) ;
#389 = CARTESIAN_POINT ( 'NONE',  ( -4.209348295687703967, -3.401574460001763001, -6.437500000000003553 ) ) ;
#390 = CARTESIAN_POINT ( 'NONE',  ( -0.5636800770129166693, -4.293361309317430319, -3.531542292955206275 ) ) ;
#391 = CARTESIAN_POINT ( 'NONE',  ( -4.458734125000001214, -22.87500000136559564, 1.846868145590734089 ) ) ;
#392 = CARTESIAN_POINT ( 'NONE',  ( -3.753672977998669946, -3.033343224707661712, -7.999999998634409692 ) ) ;
#393 = EDGE_LOOP ( 'NONE', ( #15689, #8043, #13858, #8283 ) ) ;
#394 = DIRECTION ( 'NONE',  ( -0.000000000000000000, -1.000000000000000000, -0.000000000000000000 ) ) ;
#395 = VERTEX_POINT ( 'NONE', #15166 ) ;
#396 = SHAPE_REPRESENTATION ( 'Synchronized Concentric Jaws', ( #3223 ), #1155 ) ;
#397 = ORIENTED_EDGE ( 'NONE', *, *, #8592, .F. ) ;
#398 = STYLED_ITEM ( 'NONE', ( #7612 ), #14732 ) ;
#399 = CARTESIAN_POINT ( 'NONE',  ( 3.152801135295367541, -31.56250000136559564, -3.152801135295367541 ) ) ;
#400 = EDGE_CURVE ( 'NONE', #3541, #15546, #10896, .T. ) ;
#401 = CARTESIAN_POINT ( 'NONE',  ( 0.000000000000000000, -32.00000000000000000, 0.000000000000000000 ) ) ;
#402 = EDGE_CURVE ( 'NONE', #3787, #10893, #14404, .T. ) ;
#403 = CIRCLE ( 'NONE', #1678, 25.00000000000000000 ) ;
#404 = ORIENTED_EDGE ( 'NONE', *, *, #14622, .T. ) ;
#405 = CARTESIAN_POINT ( 'NONE',  ( -0.1404048886732797152, -4.699864953788083888, -3.686887068327043160 ) ) ;
#406 = DIRECTION ( 'NONE',  ( -0.000000000000000000, -1.000000000000000000, -0.000000000000000000 ) ) ;
#407 = CARTESIAN_POINT ( 'NONE',  ( 3.033343224707661712, -3.753672977998669502, -1.499999998634408138 ) ) ;
#408 = CARTESIAN_POINT ( 'NONE',  ( 4.458734125001844184, 0.2692756610531124029, -0.3789984458506765463 ) ) ;
#409 = CARTESIAN_POINT ( 'NONE',  ( 5.000000000000000000, -29.06250000000000000, 2.071067811865478614 ) ) ;
#410 =( GEOMETRIC_REPRESENTATION_CONTEXT ( 3 ) GLOBAL_UNCERTAINTY_ASSIGNED_CONTEXT ( ( #3205 ) ) GLOBAL_UNIT_ASSIGNED_CONTEXT ( ( #8747, #1452, #4035 ) ) REPRESENTATION_CONTEXT ( 'NONE', 'WORKASPACE' ) );
#411 = CARTESIAN_POINT ( 'NONE',  ( -2.000000000000007550, -3.464101615137749945, 0.000000000000000000 ) ) ;
#412 = DIRECTION ( 'NONE',  ( 0.000000000000000000, 0.000000000000000000, 1.000000000000000000 ) ) ;
#413 = CARTESIAN_POINT ( 'NONE',  ( -3.535533905932738641, -24.50000000273118772, 3.535533905932737309 ) ) ;
#414 = AXIS2_PLACEMENT_3D ( 'NONE', #3644, #8589, #5995 ) ;
#415 = PLANE ( 'NONE',  #1616 ) ;
#416 = CARTESIAN_POINT ( 'NONE',  ( 4.458734124999999437, -26.37500000136559564, -1.846868145590734978 ) ) ;
#417 = CARTESIAN_POINT ( 'NONE',  ( -35.00000000000000000, 40.00000000000000000, 0.000000000000000000 ) ) ;
#418 = ORIENTED_EDGE ( 'NONE', *, *, #14329, .F. ) ;
#419 = ORIENTED_EDGE ( 'NONE', *, *, #12438, .F. ) ;
#420 = ORIENTED_EDGE ( 'NONE', *, *, #9806, .F. ) ;
#421 = CARTESIAN_POINT ( 'NONE',  ( -44.05158835363087633, -3.098194602941751530, 21.36784885013319624 ) ) ;
#422 = ADVANCED_FACE ( 'NONE', ( #15007 ), #3921, .T. ) ;
#423 = AXIS2_PLACEMENT_3D ( 'NONE', #12972, #1755, #11374 ) ;
#424 = EDGE_LOOP ( 'NONE', ( #12881, #12363, #14774, #7098 ) ) ;
#425 = DIRECTION ( 'NONE',  ( -1.000000000000000000, 0.000000000000000000, 0.000000000000000000 ) ) ;
#426 = CIRCLE ( 'NONE', #9451, 2.649999999999985700 ) ;
#427 = DIRECTION ( 'NONE',  ( 0.000000000000000000, 1.000000000000000000, 0.000000000000000000 ) ) ;
#428 = CARTESIAN_POINT ( 'NONE',  ( 1.846868145590735200, -30.50000000136559919, -4.458734125000000326 ) ) ;
#429 = CARTESIAN_POINT ( 'NONE',  ( -1.415196051561583790, 4.795541693661363958, -0.6249999972688171646 ) ) ;
#430 = APPLICATION_PROTOCOL_DEFINITION ( 'draft international standard', 'automotive_design', 1998, #12991 ) ;
#431 = CARTESIAN_POINT ( 'NONE',  ( 0.000000000000000000, 0.000000000000000000, -25.03750572909317285 ) ) ;
#432 = CARTESIAN_POINT ( 'NONE',  ( 4.729367062499999719, -31.84375000068279959, 0.000000000000000000 ) ) ;
#433 = ORIENTED_EDGE ( 'NONE', *, *, #4049, .T. ) ;
#434 = VERTEX_POINT ( 'NONE', #14346 ) ;
#435 = LINE ( 'NONE', #9087, #7748 ) ;
#436 = CARTESIAN_POINT ( 'NONE',  ( -4.458734124999999437, -30.93750000136559564, -5.460374474430324690E-16 ) ) ;
#437 = EDGE_CURVE ( 'NONE', #15006, #14231, #6144, .T. ) ;
#438 = B_SPLINE_CURVE_WITH_KNOTS ( 'NONE', 3,
 ( #10170, #8965, #1830, #1670, #1596, #11449, #6705, #4348, #11608 ),
 .UNSPECIFIED., .F., .F.,
 ( 4, 2, 1, 2, 4 ),
 ( 0.000000000000000000, 0.002165063509461097498, 0.004330127018922194995, 0.006495190528383292493, 0.008660254037844389990 ),
 .UNSPECIFIED. ) ;
#439 = ORIENTED_EDGE ( 'NONE', *, *, #14620, .F. ) ;
#440 = CARTESIAN_POINT ( 'NONE',  ( 3.916244202832140253, -2.131511515620588160, -7.687499998634407916 ) ) ;
#441 = CIRCLE ( 'NONE', #4826, 29.99999999999999289 ) ;
#442 = LINE ( 'NONE', #15389, #913 ) ;
#443 = ORIENTED_EDGE ( 'NONE', *, *, #6817, .F. ) ;
#444 = CIRCLE ( 'NONE', #3775, 5.560781378645573980 ) ;
#445 = CARTESIAN_POINT ( 'NONE',  ( -3.535533905932737309, -28.75000000273118772, -3.535533905932738197 ) ) ;
#446 = EDGE_CURVE ( 'NONE', #12836, #3368, #3237, .T. ) ;
#447 = DIRECTION ( 'NONE',  ( 0.000000000000000000, 0.000000000000000000, 1.000000000000000000 ) ) ;
#448 = UNCERTAINTY_MEASURE_WITH_UNIT (LENGTH_MEASURE( 1.000000000000000082E-05 ), #1256, 'distance_accuracy_value', 'NONE');
#449 = CARTESIAN_POINT ( 'NONE',  ( -1.415196051561583790, 4.795541693661363958, -2.624999997268815388 ) ) ;
#450 = CARTESIAN_POINT ( 'NONE',  ( -4.999999999999847233, 1.272547481429013860, -8.461597479913463005 ) ) ;
#451 = ADVANCED_FACE ( 'NONE', ( #852 ), #7980, .T. ) ;
#452 = AXIS2_PLACEMENT_3D ( 'NONE', #5371, #14093, #447 ) ;
#453 = CARTESIAN_POINT ( 'NONE',  ( 3.152801135295367541, -23.56250000136559564, -3.152801135295367541 ) ) ;
#454 = ORIENTED_EDGE ( 'NONE', *, *, #5990, .F. ) ;
#455 = FACE_BOUND ( 'NONE', #11569, .T. ) ;
#456 = PLANE ( 'NONE',  #8190 ) ;
#457 = CARTESIAN_POINT ( 'NONE',  ( -2.500000000000000444, 3.061616997868383634E-16, -25.03750572909317285 ) ) ;
#458 = ORIENTED_EDGE ( 'NONE', *, *, #13196, .F. ) ;
#459 = CYLINDRICAL_SURFACE ( 'NONE', #12090, 4.250000000000000000 ) ;
#460 = EDGE_LOOP ( 'NONE', ( #1578, #12472, #3436, #12198 ) ) ;
#461 = ORIENTED_EDGE ( 'NONE', *, *, #7687, .F. ) ;
#462 = CYLINDRICAL_SURFACE ( 'NONE', #5357, 75.00000000000001421 ) ;
#463 = CARTESIAN_POINT ( 'NONE',  ( -1.360585162435467455, 4.061296242128285883, -3.505054077164959203 ) ) ;
#464 =( BOUNDED_CURVE ( )  B_SPLINE_CURVE ( 2, ( #5096, #12595, #1539, #6477, #12273, #177, #13559, #9939, #5254, #10191, #8585, #11390, #3640, #13806, #11315, #2658, #13474, #3714, #1368, #10032, #8661, #14967, #11084, #13650, #3882, #14877, #8901, #7611, #2741, #2411, #2579, #6158, #7531, #7454, #17, #4935, #12359, #12432, #15041, #1291, #8824, #12510, #6236, #11152, #265, #13725, #1451, #5010, #15363, #6792, #8985, #12990, #6636, #5424, #14147, #9068, #4372, #6553, #3076, #5661, #1695, #15207, #1612, #15451, #1927, #4120, #11550, #4034, #6877, #13898, #11468, #10427, #14227, #5497, #576, #7936, #12915, #7853, #11782, #4285, #12670, #416, #15113, #9305, #10278, #2826, #736, #7780, #4197, #11626, #3151, #9223, #8096, #8018, #11700, #1849, #504, #9144, #5339, #13970, #2902, #12750, #2984, #10356, #15283, #14057, #12833, #1777, #655, #5581, #6725, #10517, #810, #8263, #7406, #13156, #5730, #5809, #14834, #8701, #6110, #13603, #2090, #887, #9821, #4518, #52, #2013, #14750, #1328, #7035, #11935, #7323, #12310, #3600, #9453, #12227, #10665, #1249, #7489, #15600, #11037, #9895, #1166, #11027, #8547, #8620, #3311, #12392, #4896, #8175, #10601, #2451, #13435, #6197, #10745, #15525, #4968, #11114, #15681, #4441 ),
 .UNSPECIFIED., .F., .F. ) 
 B_SPLINE_CURVE_WITH_KNOTS ( ( 3, 2, 2, 2, 2, 2, 2, 2, 2, 2, 2, 2, 2, 2, 2, 2, 2, 2, 2, 2, 2, 2, 2, 2, 2, 2, 2, 2, 2, 2, 2, 2, 2, 2, 2, 2, 2, 2, 2, 2, 2, 2, 2, 2, 2, 2, 2, 2, 2, 2, 2, 2, 2, 2, 2, 2, 2, 2, 2, 2, 2, 2, 2, 2, 2, 2, 2, 2, 2, 2, 2, 2, 2, 2, 2, 2, 2, 2, 2, 2, 3 ),
 ( 0.000000000000000000, 0.01250000000000000069, 0.02500000000000000139, 0.03749999999999999861, 0.05000000000000000278, 0.06250000000000000000, 0.07499999999999999722, 0.08749999999999999445, 0.1000000000000000056, 0.1125000000000000028, 0.1250000000000000000, 0.1375000000000000111, 0.1499999999999999944, 0.1625000000000000056, 0.1749999999999999889, 0.1875000000000000000, 0.2000000000000000111, 0.2124999999999999944, 0.2250000000000000056, 0.2374999999999999889, 0.2500000000000000000, 0.2625000000000000111, 0.2750000000000000222, 0.2874999999999999778, 0.2999999999999999889, 0.3125000000000000000, 0.3250000000000000111, 0.3375000000000000222, 0.3499999999999999778, 0.3624999999999999889, 0.3750000000000000000, 0.3875000000000000111, 0.4000000000000000222, 0.4124999999999999778, 0.4249999999999999889, 0.4375000000000000000, 0.4500000000000000111, 0.4625000000000000222, 0.4749999999999999778, 0.4874999999999999889, 0.5000000000000000000, 0.5124999999999999556, 0.5250000000000000222, 0.5374999999999999778, 0.5500000000000000444, 0.5625000000000000000, 0.5749999999999999556, 0.5875000000000000222, 0.5999999999999999778, 0.6125000000000000444, 0.6250000000000000000, 0.6374999999999999556, 0.6500000000000000222, 0.6624999999999999778, 0.6750000000000000444, 0.6875000000000000000, 0.6999999999999999556, 0.7125000000000000222, 0.7249999999999999778, 0.7375000000000000444, 0.7500000000000000000, 0.7624999999999999556, 0.7750000000000000222, 0.7874999999999999778, 0.8000000000000000444, 0.8125000000000000000, 0.8249999999999999556, 0.8375000000000000222, 0.8499999999999999778, 0.8625000000000000444, 0.8750000000000000000, 0.8874999999999999556, 0.9000000000000000222, 0.9124999999999999778, 0.9250000000000000444, 0.9375000000000000000, 0.9499999999999999556, 0.9625000000000000222, 0.9749999999999999778, 0.9875000000000000444, 1.000000000000000000 ),
 .UNSPECIFIED. ) 
 CURVE ( )  GEOMETRIC_REPRESENTATION_ITEM ( )  RATIONAL_B_SPLINE_CURVE ( ( 1.000000000000000000, 0.9238795325112867385, 1.000000000000000000, 0.9238795325112867385, 1.000000000000000000, 0.9238795325112867385, 1.000000000000000000, 0.9238795325112867385, 1.000000000000000000, 0.9238795325112867385, 1.000000000000000000, 0.9238795325112867385, 1.000000000000000000, 0.9238795325112867385, 1.000000000000000000, 0.9238795325112867385, 1.000000000000000000, 0.9238795325112867385, 1.000000000000000000, 0.9238795325112867385, 1.000000000000000000, 0.9238795325112867385, 1.000000000000000000, 0.9238795325112867385, 1.000000000000000000, 0.9238795325112867385, 1.000000000000000000, 0.9238795325112867385, 1.000000000000000000, 0.9238795325112867385, 1.000000000000000000, 0.9238795325112867385, 1.000000000000000000, 0.9238795325112867385, 1.000000000000000000, 0.9238795325112867385, 1.000000000000000000, 0.9238795325112867385, 1.000000000000000000, 0.9238795325112867385, 1.000000000000000000, 0.9238795325112867385, 1.000000000000000000, 0.9238795325112867385, 1.000000000000000000, 0.9238795325112867385, 1.000000000000000000, 0.9238795325112867385, 1.000000000000000000, 0.9238795325112867385, 1.000000000000000000, 0.9238795325112867385, 1.000000000000000000, 0.9238795325112867385, 1.000000000000000000, 0.9238795325112867385, 1.000000000000000000, 0.9238795325112867385, 1.000000000000000000, 0.9238795325112867385, 1.000000000000000000, 0.9238795325112867385, 1.000000000000000000, 0.9238795325112867385, 1.000000000000000000, 0.9238795325112867385, 1.000000000000000000, 0.9238795325112867385, 1.000000000000000000, 0.9238795325112867385, 1.000000000000000000, 0.9238795325112867385, 1.000000000000000000, 0.9238795325112867385, 1.000000000000000000, 0.9238795325112867385, 1.000000000000000000, 0.9238795325112867385, 1.000000000000000000, 0.9238795325112867385, 1.000000000000000000, 0.9238795325112867385, 1.000000000000000000, 0.9238795325112867385, 1.000000000000000000, 0.9238795325112867385, 1.000000000000000000, 0.9238795325112867385, 1.000000000000000000, 0.9238795325112867385, 1.000000000000000000, 0.9238795325112867385, 1.000000000000000000, 0.9238795325112867385, 1.000000000000000000, 0.9238795325112867385, 1.000000000000000000, 0.9238795325112867385, 1.000000000000000000, 0.9238795325112867385, 1.000000000000000000, 0.9238795325112867385, 1.000000000000000000, 0.9238795325112867385, 1.000000000000000000, 0.9238795325112867385, 1.000000000000000000, 0.9238795325112867385, 1.000000000000000000, 0.9238795325112867385, 1.000000000000000000, 0.9238795325112867385, 1.000000000000000000, 0.9238795325112867385, 1.000000000000000000, 0.9238795325112867385, 1.000000000000000000, 0.9238795325112867385, 1.000000000000000000, 0.9238795325112867385, 1.000000000000000000, 0.9238795325112867385, 1.000000000000000000, 0.9238795325112867385, 1.000000000000000000, 0.9238795325112867385, 1.000000000000000000, 0.9238795325112867385, 1.000000000000000000, 0.9238795325112867385, 1.000000000000000000, 0.9238795325112867385, 1.000000000000000000, 0.9238795325112867385, 1.000000000000000000, 0.9238795325112867385, 1.000000000000000000, 0.9238795325112867385, 1.000000000000000000, 0.9238795325112867385, 1.000000000000000000, 0.9238795325112867385, 1.000000000000000000, 0.9238795325112867385, 1.000000000000000000, 0.9238795325112867385, 1.000000000000000000, 0.9238795325112867385, 1.000000000000000000, 0.9238795325112867385, 1.000000000000000000, 0.9238795325112867385, 1.000000000000000000, 0.9238795325112867385, 1.000000000000000000, 0.9238795325112867385, 1.000000000000000000, 0.9238795325112867385, 1.000000000000000000, 0.9238795325112867385, 1.000000000000000000 ) ) 
 REPRESENTATION_ITEM ( '' )  );
#465 = DIRECTION ( 'NONE',  ( 8.673617379884034486E-16, 0.000000000000000000, 1.000000000000000000 ) ) ;
#466 = AXIS2_PLACEMENT_3D ( 'NONE', #5707, #10643, #4493 ) ;
#467 = DIRECTION ( 'NONE',  ( -1.000000000000000000, -0.000000000000000000, -0.000000000000000000 ) ) ;
#468 = FACE_BOUND ( 'NONE', #14883, .T. ) ;
#469 = FACE_OUTER_BOUND ( 'NONE', #10752, .T. ) ;
#470 = AXIS2_PLACEMENT_3D ( 'NONE', #10148, #3841, #13765 ) ;
#471 = CARTESIAN_POINT ( 'NONE',  ( 2.390265326283148806, 4.391654775818395251, -5.875000000000001776 ) ) ;
#472 = DIRECTION ( 'NONE',  ( 0.000000000000000000, -1.000000000000000000, 0.000000000000000000 ) ) ;
#473 = EDGE_CURVE ( 'NONE', #8001, #6278, #15322, .T. ) ;
#474 = CARTESIAN_POINT ( 'NONE',  ( -6.902527771671635115, -4.675077770780904807, -0.7026937717022864183 ) ) ;
#475 = EDGE_CURVE ( 'NONE', #1675, #4627, #623, .T. ) ;
#476 = CARTESIAN_POINT ( 'NONE',  ( 1.846868145590735200, -24.25000000136559564, -4.458734125000000326 ) ) ;
#477 = CARTESIAN_POINT ( 'NONE',  ( -1.261996585732579224, 4.276409079477648589, -7.312499998634407916 ) ) ;
#478 = EDGE_LOOP ( 'NONE', ( #2495, #13300, #2111, #13302 ) ) ;
#479 = UNCERTAINTY_MEASURE_WITH_UNIT (LENGTH_MEASURE( 1.000000000000000082E-05 ), #11657, 'distance_accuracy_value', 'NONE');
#480 = VECTOR ( 'NONE', #9120, 1000.000000000000000 ) ;
#481 = DIRECTION ( 'NONE',  ( 0.000000000000000000, 0.000000000000000000, 1.000000000000000000 ) ) ;
#482 = VERTEX_POINT ( 'NONE', #13120 ) ;
#483 = ORIENTED_EDGE ( 'NONE', *, *, #15732, .F. ) ;
#484 = ORIENTED_EDGE ( 'NONE', *, *, #9626, .T. ) ;
#485 = CARTESIAN_POINT ( 'NONE',  ( 1.846868145590736310, -21.62500000136559564, 4.458734124999999437 ) ) ;
#486 = DIRECTION ( 'NONE',  ( -1.387778780781446464E-15, -1.000000000000000000, 1.387778780781447648E-15 ) ) ;
#487 = ORIENTED_EDGE ( 'NONE', *, *, #7096, .T. ) ;
#488 = DIRECTION ( 'NONE',  ( 0.000000000000000000, -0.000000000000000000, 1.000000000000000000 ) ) ;
#489 = CARTESIAN_POINT ( 'NONE',  ( 7.500000000000000000, 4.732328341851992803, -7.493855119309153601 ) ) ;
#490 = CARTESIAN_POINT ( 'NONE',  ( -0.5093500532425060401, -4.799145180956616130, -2.624999998634407028 ) ) ;
#491 = DIRECTION ( 'NONE',  ( 0.000000000000000000, 1.000000000000000000, 0.000000000000000000 ) ) ;
#492 = AXIS2_PLACEMENT_3D ( 'NONE', #7401, #13083, #5207 ) ;
#493 = AXIS2_PLACEMENT_3D ( 'NONE', #9026, #13762, #300 ) ;
#494 = CARTESIAN_POINT ( 'NONE',  ( 2.071067811865476394, -26.18750000000000355, 5.000000000000000000 ) ) ;
#495 = CARTESIAN_POINT ( 'NONE',  ( 3.033343224707661712, -3.753672977998669946, -5.499999998634407916 ) ) ;
#496 = CARTESIAN_POINT ( 'NONE',  ( -7.500000000000000000, -4.330127018922196314, -7.422398894150035176 ) ) ;
#497 = VECTOR ( 'NONE', #7170, 1000.000000000000000 ) ;
#498 = DIRECTION ( 'NONE',  ( 1.000000000000000000, 0.000000000000000000, 0.000000000000000000 ) ) ;
#499 = EDGE_CURVE ( 'NONE', #2433, #13770, #15943, .T. ) ;
#500 = CARTESIAN_POINT ( 'NONE',  ( -2.071067811865475061, -24.81250000273118417, -5.000000000000000888 ) ) ;
#501 = PRODUCT_DEFINITION ( 'UNKNOWN', '', #14374, #14001 ) ;
#502 = DIRECTION ( 'NONE',  ( 1.000000000000000000, 0.000000000000000000, 0.000000000000000000 ) ) ;
#503 = CIRCLE ( 'NONE', #4355, 5.000000000000000000 ) ;
#504 = CARTESIAN_POINT ( 'NONE',  ( 4.458734124999999437, -25.43750000136559564, 0.000000000000000000 ) ) ;
#505 = CARTESIAN_POINT ( 'NONE',  ( 5.276498195232060873, -6.073236878018049900, -7.633618187056725901 ) ) ;
#506 = ORIENTED_EDGE ( 'NONE', *, *, #4910, .T. ) ;
#507 = EDGE_LOOP ( 'NONE', ( #8212, #12137, #15528 ) ) ;
#508 = CARTESIAN_POINT ( 'NONE',  ( 7.500000000000001776, 0.000000000000000000, 0.000000000000000000 ) ) ;
#509 = VERTEX_POINT ( 'NONE', #3119 ) ;
#510 = CYLINDRICAL_SURFACE ( 'NONE', #2443, 3.499999999999999556 ) ;
#511 = AXIS2_PLACEMENT_3D ( 'NONE', #3359, #10867, #8309 ) ;
#512 = VECTOR ( 'NONE', #11630, 1000.000000000000000 ) ;
#513 = VERTEX_POINT ( 'NONE', #14500 ) ;
#514 = CARTESIAN_POINT ( 'NONE',  ( 2.143131898507869826E-15, 40.00000000000000000, -64.85000000000002274 ) ) ;
#515 = CARTESIAN_POINT ( 'NONE',  ( 0.000000000000000000, 37.00000000000000000, 75.00000000000001421 ) ) ;
#516 = CARTESIAN_POINT ( 'NONE',  ( 47.32050807568879947, -37.00000000000000711, -41.96152422706630603 ) ) ;
#517 = DIRECTION ( 'NONE',  ( 1.000000000000000000, -0.000000000000000000, -1.239088197126290570E-16 ) ) ;
#518 = ADVANCED_FACE ( 'NONE', ( #10565 ), #8302, .F. ) ;
#519 = ADVANCED_FACE ( 'NONE', ( #932 ), #7080, .T. ) ;
#520 = EDGE_CURVE ( 'NONE', #13539, #6761, #9245, .T. ) ;
#521 = EDGE_CURVE ( 'NONE', #13476, #13669, #12188, .T. ) ;
#522 = VECTOR ( 'NONE', #25, 1000.000000000000000 ) ;
#523 = FACE_OUTER_BOUND ( 'NONE', #7763, .T. ) ;
#524 = ORIENTED_EDGE ( 'NONE', *, *, #6442, .T. ) ;
#525 =( NAMED_UNIT ( * ) SI_UNIT ( $, .STERADIAN. ) SOLID_ANGLE_UNIT ( ) );
#526 = EDGE_LOOP ( 'NONE', ( #2721, #11527, #12496, #1351, #6317, #10390, #12512 ) ) ;
#527 = CARTESIAN_POINT ( 'NONE',  ( 9.999999999999891642, -13.00000000000000178, -17.32050807568883499 ) ) ;
#528 = CARTESIAN_POINT ( 'NONE',  ( -4.458734125000001214, -27.87500000136559564, 1.846868145590734089 ) ) ;
#529 = ORIENTED_EDGE ( 'NONE', *, *, #6898, .T. ) ;
#530 = CONTEXT_DEPENDENT_SHAPE_REPRESENTATION ( #11050, #13975 ) ;
#531 = CARTESIAN_POINT ( 'NONE',  ( 0.000000000000000000, 0.000000000000000000, 0.000000000000000000 ) ) ;
#532 = CARTESIAN_POINT ( 'NONE',  ( 5.000000000000002665, 1.275685995473128912E-14, -4.920263044861760804 ) ) ;
#533 = CARTESIAN_POINT ( 'NONE',  ( 4.391654775818395251, -2.390265326283149694, -7.999999997268813168 ) ) ;
#534 = EDGE_CURVE ( 'NONE', #9400, #9517, #9860, .T. ) ;
#535 = CARTESIAN_POINT ( 'NONE',  ( -4.795541693661363958, -1.415196051561583790, -8.374999997268814056 ) ) ;
#536 = DIRECTION ( 'NONE',  ( -0.8660254037844388186, -0.000000000000000000, 0.4999999999999998890 ) ) ;
#537 =( REPRESENTATION_RELATIONSHIP ('NONE','NONE', #4176, #10906 ) REPRESENTATION_RELATIONSHIP_WITH_TRANSFORMATION ( #2604 )SHAPE_REPRESENTATION_RELATIONSHIP( ) );
#538 = CARTESIAN_POINT ( 'NONE',  ( -4.458734124999999437, -23.18750000136559564, -5.460374474430324690E-16 ) ) ;
#539 = ORIENTED_EDGE ( 'NONE', *, *, #227, .F. ) ;
#540 = FACE_OUTER_BOUND ( 'NONE', #7813, .T. ) ;
#541 = CARTESIAN_POINT ( 'NONE',  ( 3.753672977998667726, 3.033343224707664376, -8.249999998634409692 ) ) ;
#542 = CARTESIAN_POINT ( 'NONE',  ( 5.000000000000004441, 6.350331166892669572E-15, -1.045263047592943417 ) ) ;
#543 = ORIENTED_EDGE ( 'NONE', *, *, #4679, .T. ) ;
#544 = CARTESIAN_POINT ( 'NONE',  ( -67.50000000000000000, 40.00000000000000000, -7.070249711157346244E-13 ) ) ;
#545 = ORIENTED_EDGE ( 'NONE', *, *, #14696, .T. ) ;
#546 = ORIENTED_EDGE ( 'NONE', *, *, #11089, .F. ) ;
#547 = CARTESIAN_POINT ( 'NONE',  ( -7.922281120364393914, 4.573931137438272287, -8.047472243342932430 ) ) ;
#548 = CARTESIAN_POINT ( 'NONE',  ( 0.000000000000000000, -20.00000000000000000, 0.000000000000000000 ) ) ;
#549 = FACE_OUTER_BOUND ( 'NONE', #2959, .T. ) ;
#550 = CYLINDRICAL_SURFACE ( 'NONE', #13850, 2.649999999999992806 ) ;
#551 = DIRECTION ( 'NONE',  ( -0.000000000000000000, 1.000000000000000000, -0.000000000000000000 ) ) ;
#552 = CARTESIAN_POINT ( 'NONE',  ( 5.000000000000000000, -23.06250000000000000, 2.071067811865478614 ) ) ;
#553 = CARTESIAN_POINT ( 'NONE',  ( -5.381735091635034607, 0.5711823568785950878, -7.562500000000005329 ) ) ;
#554 = FACE_OUTER_BOUND ( 'NONE', #8051, .T. ) ;
#555 = CARTESIAN_POINT ( 'NONE',  ( 5.000000000000000888, -25.06250000273118417, -2.071067811865475505 ) ) ;
#556 = FACE_OUTER_BOUND ( 'NONE', #7798, .T. ) ;
#557 = CARTESIAN_POINT ( 'NONE',  ( -2.131511515620587272, -3.916244202832140253, -5.937499998634407028 ) ) ;
#558 = EDGE_LOOP ( 'NONE', ( #4178, #10902, #2223, #13257 ) ) ;
#559 = LINE ( 'NONE', #10495, #3498 ) ;
#560 = VERTEX_POINT ( 'NONE', #14792 ) ;
#561 = ORIENTED_EDGE ( 'NONE', *, *, #4255, .T. ) ;
#562 = CARTESIAN_POINT ( 'NONE',  ( 1.846868145590736310, -30.87500000136559564, 4.458734124999999437 ) ) ;
#563 = LINE ( 'NONE', #9209, #9705 ) ;
#564 = ORIENTED_EDGE ( 'NONE', *, *, #15075, .T. ) ;
#565 = CARTESIAN_POINT ( 'NONE',  ( -5.000000000000092371, -0.7223674278660636716, -6.521799365517155778 ) ) ;
#566 = EDGE_CURVE ( 'NONE', #15546, #13370, #8395, .T. ) ;
#567 = FACE_OUTER_BOUND ( 'NONE', #4201, .T. ) ;
#568 = CARTESIAN_POINT ( 'NONE',  ( -3.916244202832140253, 2.131511515620587272, -3.937499998634404808 ) ) ;
#569 = DIRECTION ( 'NONE',  ( -0.000000000000000000, -1.000000000000000000, -0.000000000000000000 ) ) ;
#570 = CARTESIAN_POINT ( 'NONE',  ( -5.000000000000000000, -27.50000000000000000, -6.123233995736766282E-16 ) ) ;
#571 = CARTESIAN_POINT ( 'NONE',  ( -2.131511515620587272, -3.916244202832140253, -5.687499998634406140 ) ) ;
#572 = DIRECTION ( 'NONE',  ( 0.000000000000000000, 0.000000000000000000, 1.000000000000000000 ) ) ;
#573 = DIRECTION ( 'NONE',  ( 0.000000000000000000, 1.000000000000000000, 0.000000000000000000 ) ) ;
#574 = CARTESIAN_POINT ( 'NONE',  ( 5.000000000000000000, -23.18750000273119127, 2.071067811865478614 ) ) ;
#575 = CARTESIAN_POINT ( 'NONE',  ( 31.75426480542942898, -4.999999999999997335, -14.99999999999999645 ) ) ;
#576 = CARTESIAN_POINT ( 'NONE',  ( -3.152801135295367985, -26.81250000136559564, 3.152801135295367096 ) ) ;
#577 = ORIENTED_EDGE ( 'NONE', *, *, #4143, .F. ) ;
#578 = ORIENTED_EDGE ( 'NONE', *, *, #400, .F. ) ;
#579 = CARTESIAN_POINT ( 'NONE',  ( 3.511755186886750923, -2.826662030176382956, -3.597382984111582083 ) ) ;
#580 = VERTEX_POINT ( 'NONE', #7452 ) ;
#581 = CARTESIAN_POINT ( 'NONE',  ( -43.85680617780057844, -3.000000000000000000, 22.00000000000000355 ) ) ;
#582 = VECTOR ( 'NONE', #7048, 1000.000000000000000 ) ;
#583 = ORIENTED_EDGE ( 'NONE', *, *, #907, .F. ) ;
#584 = DIRECTION ( 'NONE',  ( 0.000000000000000000, 1.000000000000000000, 0.000000000000000000 ) ) ;
#585 = EDGE_CURVE ( 'NONE', #1848, #15683, #12358, .T. ) ;
#586 = EDGE_CURVE ( 'NONE', #13829, #5811, #14718, .T. ) ;
#587 = LINE ( 'NONE', #1466, #12695 ) ;
#588 = CARTESIAN_POINT ( 'NONE',  ( -3.152801135295367985, -26.06250000136559919, 3.152801135295367096 ) ) ;
#589 = CARTESIAN_POINT ( 'NONE',  ( 2.390265326283148806, 4.391654775818395251, -5.875000000000001776 ) ) ;
#590 = CARTESIAN_POINT ( 'NONE',  ( -5.000000000000092371, -0.7223674278660648929, -0.3967993627859714989 ) ) ;
#591 = CARTESIAN_POINT ( 'NONE',  ( 4.799145180956616130, -0.5093500532425063732, -7.624999998634408804 ) ) ;
#592 = LINE ( 'NONE', #12766, #15405 ) ;
#593 = AXIS2_PLACEMENT_3D ( 'NONE', #15441, #2156, #1919 ) ;
#594 = EDGE_LOOP ( 'NONE', ( #1579, #15115, #2346, #7475 ) ) ;
#595 = FILL_AREA_STYLE_COLOUR ( '', #11712 ) ;
#596 = ORIENTED_EDGE ( 'NONE', *, *, #12479, .T. ) ;
#597 = DIRECTION ( 'NONE',  ( 1.000000000000000000, 1.239088197126290324E-16, -0.000000000000000000 ) ) ;
#598 = ORIENTED_EDGE ( 'NONE', *, *, #1280, .F. ) ;
#599 = CONTEXT_DEPENDENT_SHAPE_REPRESENTATION ( #6618, #5471 ) ;
#600 = EDGE_CURVE ( 'NONE', #4642, #13521, #7060, .T. ) ;
#601 = EDGE_CURVE ( 'NONE', #3228, #2810, #2578, .T. ) ;
#602 = CIRCLE ( 'NONE', #5747, 2.649999999999985700 ) ;
#603 = DIRECTION ( 'NONE',  ( -1.000000000000000000, 0.000000000000000000, 1.239088197126290570E-16 ) ) ;
#604 = CIRCLE ( 'NONE', #12193, 3.499999999999999556 ) ;
#605 = CARTESIAN_POINT ( 'NONE',  ( 4.391654775818395251, -2.390265326283149694, -2.999999997268815832 ) ) ;
#606 = CARTESIAN_POINT ( 'NONE',  ( 3.061616997868383043E-15, -13.00000000000000178, 25.00000000000000000 ) ) ;
#607 = UNCERTAINTY_MEASURE_WITH_UNIT (LENGTH_MEASURE( 1.000000000000000082E-05 ), #5032, 'distance_accuracy_value', 'NONE');
#608 = ADVANCED_BREP_SHAPE_REPRESENTATION ( '', ( #9113, #3223 ), #1938 ) ;
#609 = PRODUCT ( 'Central Drive Wedge _ Scroll Plate', 'Central Drive Wedge _ Scroll Plate', '', ( #8672 ) ) ;
#611 = VECTOR ( 'NONE', #13383, 1000.000000000000000 ) ;
#610 = CARTESIAN_POINT ( 'NONE',  ( 3.401574460001763001, -4.209348295687703967, -6.062499997268814056 ) ) ;
#612 = CARTESIAN_POINT ( 'NONE',  ( 33.48631561299831105, -5.000000000000000000, -13.99999999999999645 ) ) ;
#613 = DIRECTION ( 'NONE',  ( -0.000000000000000000, 1.000000000000000000, -0.000000000000000000 ) ) ;
#614 = CARTESIAN_POINT ( 'NONE',  ( 3.061616997868383141E-16, -24.75000000000000000, -5.000000000000000000 ) ) ;
#615 = VERTEX_POINT ( 'NONE', #3712 ) ;
#616 = CARTESIAN_POINT ( 'NONE',  ( 2.500000000000000000, 0.000000000000000000, 0.000000000000000000 ) ) ;
#617 = CARTESIAN_POINT ( 'NONE',  ( -81.33974596215558961, -105.7735026918962404, 17.50000000000000000 ) ) ;
#618 = CARTESIAN_POINT ( 'NONE',  ( -17.99999999999979394, -11.00000000000000178, 1.499999999999999112 ) ) ;
#619 = EDGE_LOOP ( 'NONE', ( #15665, #842, #2905, #10808 ) ) ;
#620 = DIRECTION ( 'NONE',  ( -1.000000000000000000, -0.000000000000000000, -0.000000000000000000 ) ) ;
#621 = VERTEX_POINT ( 'NONE', #4934 ) ;
#622 = ORIENTED_EDGE ( 'NONE', *, *, #6645, .F. ) ;
#623 = LINE ( 'NONE', #9571, #6285 ) ;
#624 = CARTESIAN_POINT ( 'NONE',  ( 67.49999999999931788, 50.00000000000000000, 2.081668171172168513E-14 ) ) ;
#625 = EDGE_CURVE ( 'NONE', #8156, #9146, #15845, .T. ) ;
#626 = DIRECTION ( 'NONE',  ( 0.5000000000000002220, -8.673617379884032514E-16, -0.8660254037844383745 ) ) ;
#627 = CARTESIAN_POINT ( 'NONE',  ( 5.000000000000000888, -26.06250000273118417, -2.071067811865475505 ) ) ;
#628 = DIRECTION ( 'NONE',  ( 0.000000000000000000, 0.000000000000000000, 1.000000000000000000 ) ) ;
#629 = CARTESIAN_POINT ( 'NONE',  ( 0.000000000000000000, -13.00000000000000178, 0.000000000000000000 ) ) ;
#630 = CARTESIAN_POINT ( 'NONE',  ( -91.28042740779480368, -120.0589677227266918, -7.500000000000000000 ) ) ;
#631 = CARTESIAN_POINT ( 'NONE',  ( 2.143131898507869826E-15, 37.00000000000000000, -67.50000000000000000 ) ) ;
#632 = CARTESIAN_POINT ( 'NONE',  ( -7.500000000000000888, -4.330127018922199866, -1.000000000000000888 ) ) ;
#633 = CARTESIAN_POINT ( 'NONE',  ( -3.152801135295367985, -21.81250000136559208, 3.152801135295367096 ) ) ;
#634 = CARTESIAN_POINT ( 'NONE',  ( 2.131511515620586383, 3.916244202832140253, -0.1874999986344084990 ) ) ;
#635 = VERTEX_POINT ( 'NONE', #5988 ) ;
#636 = DIRECTION ( 'NONE',  ( 0.000000000000000000, 0.000000000000000000, 1.000000000000000000 ) ) ;
#637 = VERTEX_POINT ( 'NONE', #15936 ) ;
#638 = ORIENTED_EDGE ( 'NONE', *, *, #11162, .F. ) ;
#639 = CARTESIAN_POINT ( 'NONE',  ( -4.458734125000000326, -22.00000000136559208, -1.846868145590735644 ) ) ;
#640 = CARTESIAN_POINT ( 'NONE',  ( -4.999999999999847233, 1.272547481429013860, -7.586597482644652501 ) ) ;
#641 = EDGE_CURVE ( 'NONE', #11474, #10194, #4211, .T. ) ;
#642 = EDGE_LOOP ( 'NONE', ( #4159, #10843 ) ) ;
#643 = CARTESIAN_POINT ( 'NONE',  ( 4.391654775818395251, -2.390265326283149694, -6.125000000000001776 ) ) ;
#644 = AXIS2_PLACEMENT_3D ( 'NONE', #5171, #10099, #12584 ) ;
#645 = AXIS2_PLACEMENT_3D ( 'NONE', #6232, #7360, #12268 ) ;
#646 = DIRECTION ( 'NONE',  ( -0.000000000000000000, -1.000000000000000000, -0.000000000000000000 ) ) ;
#647 = CARTESIAN_POINT ( 'NONE',  ( -3.033343224707664820, 3.753672977998667726, -5.999999998634408804 ) ) ;
#648 = CARTESIAN_POINT ( 'NONE',  ( 0.000000000000000000, 0.000000000000000000, -25.03750572909317285 ) ) ;
#649 = CARTESIAN_POINT ( 'NONE',  ( 5.000000000000000888, -27.93750000000000711, -2.071067811865475505 ) ) ;
#650 = CARTESIAN_POINT ( 'NONE',  ( -3.033343224707664376, 3.753672977998667726, -5.999999998634407916 ) ) ;
#651 = LINE ( 'NONE', #15677, #14820 ) ;
#652 = DIRECTION ( 'NONE',  ( 0.000000000000000000, 0.000000000000000000, -1.000000000000000000 ) ) ;
#653 = CARTESIAN_POINT ( 'NONE',  ( -9.184850993605147944E-16, -23.37500000273118772, 5.000000000000000000 ) ) ;
#654 = ORIENTED_EDGE ( 'NONE', *, *, #7999, .T. ) ;
#655 = CARTESIAN_POINT ( 'NONE',  ( -8.190561711645485556E-16, -24.68750000136559564, 4.458734124999999437 ) ) ;
#656 = EDGE_CURVE ( 'NONE', #7770, #11426, #2343, .T. ) ;
#657 = CARTESIAN_POINT ( 'NONE',  ( 0.5711823568785988625, 5.381735091635026613, -6.812500000000005329 ) ) ;
#658 = VERTEX_POINT ( 'NONE', #6156 ) ;
#659 = ORIENTED_EDGE ( 'NONE', *, *, #6025, .F. ) ;
#661 = CARTESIAN_POINT ( 'NONE',  ( 4.769696007084728073, -20.00000000000000000, 1.500000000000000000 ) ) ;
#660 = VECTOR ( 'NONE', #7753, 1000.000000000000000 ) ;
#662 = CARTESIAN_POINT ( 'NONE',  ( 21.91530404931195974, -5.000000000000000000, 6.041579923271729768 ) ) ;
#663 = ORIENTED_EDGE ( 'NONE', *, *, #8419, .F. ) ;
#664 = DIRECTION ( 'NONE',  ( 0.5000000000000001110, 0.000000000000000000, -0.8660254037844384856 ) ) ;
#665 = CARTESIAN_POINT ( 'NONE',  ( -94.14213562373093680, -97.39146311738103634, 17.50000000000001421 ) ) ;
#666 = CARTESIAN_POINT ( 'NONE',  ( 3.152801135295367541, -26.56250000136559564, -3.152801135295367541 ) ) ;
#667 = CARTESIAN_POINT ( 'NONE',  ( -4.391654775818395251, 2.390265326283148806, -0.4999999972688171090 ) ) ;
#668 = DIRECTION ( 'NONE',  ( 0.000000000000000000, -0.5000000000000012212, -0.8660254037844380415 ) ) ;
#669 = DIRECTION ( 'NONE',  ( 0.000000000000000000, 0.000000000000000000, 1.000000000000000000 ) ) ;
#670 = CARTESIAN_POINT ( 'NONE',  ( 4.276409079477644148, 1.261996585732577891, 0.4375000013655920839 ) ) ;
#671 = EDGE_CURVE ( 'NONE', #11646, #7839, #3553, .T. ) ;
#673 = EDGE_CURVE ( 'NONE', #15230, #3781, #13404, .T. ) ;
#672 = ORIENTED_EDGE ( 'NONE', *, *, #6802, .T. ) ;
#674 = CIRCLE ( 'NONE', #6869, 2.649999999999985700 ) ;
#675 = ORIENTED_EDGE ( 'NONE', *, *, #4801, .F. ) ;
#676 = DIRECTION ( 'NONE',  ( 0.000000000000000000, 1.000000000000000000, -1.471414886128461471E-15 ) ) ;
#677 = VECTOR ( 'NONE', #5737, 1000.000000000000000 ) ;
#678 = VERTEX_POINT ( 'NONE', #1212 ) ;
#679 = VECTOR ( 'NONE', #15027, 1000.000000000000000 ) ;
#680 = DIRECTION ( 'NONE',  ( -0.000000000000000000, -1.000000000000000000, -0.000000000000000000 ) ) ;
#681 = AXIS2_PLACEMENT_3D ( 'NONE', #3435, #9655, #15746 ) ;
#682 = CARTESIAN_POINT ( 'NONE',  ( 39.53738644056437579, -4.865128266864617856, 28.48076211354233322 ) ) ;
#683 = CARTESIAN_POINT ( 'NONE',  ( -44.99999999999999289, -35.00000000000000000, 17.50000000000000000 ) ) ;
#684 = CIRCLE ( 'NONE', #4805, 2.000000000000000888 ) ;
#685 = CARTESIAN_POINT ( 'NONE',  ( -0.5711823568785978633, -5.381735091635035495, -8.187499997268812280 ) ) ;
#686 = SURFACE_STYLE_USAGE ( .BOTH. , #1964 ) ;
#687 = CARTESIAN_POINT ( 'NONE',  ( 0.000000000000000000, 0.000000000000000000, -5.000000000000000000 ) ) ;
#688 = EDGE_CURVE ( 'NONE', #4101, #6399, #11429, .T. ) ;
#689 = EDGE_LOOP ( 'NONE', ( #8517, #6406, #1835, #397 ) ) ;
#690 = LINE ( 'NONE', #4556, #8733 ) ;
#691 =( NAMED_UNIT ( * ) SI_UNIT ( $, .STERADIAN. ) SOLID_ANGLE_UNIT ( ) );
#692 = ORIENTED_EDGE ( 'NONE', *, *, #3560, .T. ) ;
#693 = CARTESIAN_POINT ( 'NONE',  ( 3.535533905932736864, -27.12500000000000000, 3.535533905932738641 ) ) ;
#694 = AXIS2_PLACEMENT_3D ( 'NONE', #3412, #1145, #4634 ) ;
#695 = ORIENTED_EDGE ( 'NONE', *, *, #15597, .F. ) ;
#696 = ORIENTED_EDGE ( 'NONE', *, *, #9480, .F. ) ;
#697 = DIRECTION ( 'NONE',  ( 0.000000000000000000, -1.287488025362403787E-15, -1.000000000000000000 ) ) ;
#698 = DIRECTION ( 'NONE',  ( 0.000000000000000000, 0.000000000000000000, 1.000000000000000000 ) ) ;
#699 = AXIS2_PLACEMENT_3D ( 'NONE', #5152, #6207, #10241 ) ;
#700 = CARTESIAN_POINT ( 'NONE',  ( 2.500000000000000000, 0.000000000000000000, 0.000000000000000000 ) ) ;
#701 = VECTOR ( 'NONE', #13836, 1000.000000000000000 ) ;
#702 = CARTESIAN_POINT ( 'NONE',  ( 30.02221399786052913, -35.00000000000000000, 16.00000000000000000 ) ) ;
#704 = CARTESIAN_POINT ( 'NONE',  ( -5.000000000000000000, -25.50000000000000355, -6.123233995736766282E-16 ) ) ;
#703 = TOROIDAL_SURFACE ( 'NONE', #4044, 28.00000000000000355, 2.000000000000000000 ) ;
#705 = DIRECTION ( 'NONE',  ( -1.000000000000000000, 0.000000000000000000, 0.000000000000000000 ) ) ;
#706 = DIRECTION ( 'NONE',  ( 0.000000000000000000, 0.000000000000000000, 1.000000000000000000 ) ) ;
#707 = CARTESIAN_POINT ( 'NONE',  ( -99.99999999999998579, -25.00000000000000711, 17.50000000000000000 ) ) ;
#708 = ADVANCED_FACE ( 'NONE', ( #9143 ), #8603, .F. ) ;
#709 = DIRECTION ( 'NONE',  ( -1.000000000000000000, 0.000000000000000000, 0.000000000000000000 ) ) ;
#710 = ADVANCED_FACE ( 'NONE', ( #5496 ), #11549, .F. ) ;
#711 = CARTESIAN_POINT ( 'NONE',  ( -4.458734124999999437, -28.25000000136559919, -1.846868145590735644 ) ) ;
#712 = PRODUCT_DEFINITION_FORMATION_WITH_SPECIFIED_SOURCE ( 'ANY', '', #15460, .NOT_KNOWN. ) ;
#713 = EDGE_CURVE ( 'NONE', #79, #15920, #10355, .T. ) ;
#714 = CARTESIAN_POINT ( 'NONE',  ( -3.033343224707664376, 3.753672977998667726, -0.9999999986344076941 ) ) ;
#715 = VERTEX_POINT ( 'NONE', #575 ) ;
#716 = CARTESIAN_POINT ( 'NONE',  ( -60.00000000000000000, -4.999999999999997335, 19.99999999999999289 ) ) ;
#717 = VERTEX_POINT ( 'NONE', #15361 ) ;
#718 = ORIENTED_EDGE ( 'NONE', *, *, #3664, .F. ) ;
#719 = CARTESIAN_POINT ( 'NONE',  ( -4.458734125000000326, -28.25000000136559208, -1.846868145590735644 ) ) ;
#720 = CARTESIAN_POINT ( 'NONE',  ( 6.123233995736766282E-16, -20.00000000000000000, -5.000000000000000000 ) ) ;
#721 = VECTOR ( 'NONE', #9973, 1000.000000000000114 ) ;
#722 = CYLINDRICAL_SURFACE ( 'NONE', #11218, 10.00000000000000000 ) ;
#723 = APPLICATION_CONTEXT ( 'automotive_design' ) ;
#724 = AXIS2_PLACEMENT_3D ( 'NONE', #13932, #9982, #2858 ) ;
#725 = CARTESIAN_POINT ( 'NONE',  ( 7.500000000000698996, -1.614186302713965571, -7.450236204328873235 ) ) ;
#726 = CARTESIAN_POINT ( 'NONE',  ( 3.753672977998667726, 3.033343224707664820, -4.249999998634407028 ) ) ;
#727 = DIRECTION ( 'NONE',  ( -0.000000000000000000, -1.000000000000000000, -0.000000000000000000 ) ) ;
#728 = CARTESIAN_POINT ( 'NONE',  ( 5.000000000000000000, -24.00000000000000000, 0.000000000000000000 ) ) ;
#729 = CARTESIAN_POINT ( 'NONE',  ( -1.261996585732579224, 4.276409079477648589, -6.062499998634407028 ) ) ;
#730 = DIRECTION ( 'NONE',  ( 0.000000000000000000, 0.000000000000000000, -1.000000000000000000 ) ) ;
#731 = CIRCLE ( 'NONE', #9748, 32.00000000000000000 ) ;
#732 = CARTESIAN_POINT ( 'NONE',  ( 2.500000000000000444, 0.000000000000000000, -25.03750572909317285 ) ) ;
#733 = CARTESIAN_POINT ( 'NONE',  ( 5.000000000000000000, -21.18750000273119127, 2.071067811865478614 ) ) ;
#734 = EDGE_CURVE ( 'NONE', #8265, #3643, #11314, .T. ) ;
#735 = ORIENTED_EDGE ( 'NONE', *, *, #13938, .F. ) ;
#736 = CARTESIAN_POINT ( 'NONE',  ( -3.152801135295367096, -26.06250000136559564, -3.152801135295367541 ) ) ;
#737 = DIRECTION ( 'NONE',  ( -0.000000000000000000, -1.000000000000000000, -0.000000000000000000 ) ) ;
#738 = EDGE_LOOP ( 'NONE', ( #9185, #775, #5500, #912 ) ) ;
#739 = VERTEX_POINT ( 'NONE', #11389 ) ;
#740 = LINE ( 'NONE', #12919, #14172 ) ;
#741 = AXIS2_PLACEMENT_3D ( 'NONE', #14902, #12451, #7471 ) ;
#742 = VERTEX_POINT ( 'NONE', #5180 ) ;
#743 = CARTESIAN_POINT ( 'NONE',  ( -55.00000000000000000, -5.000000000000000000, -20.00000000000000711 ) ) ;
#744 = AXIS2_PLACEMENT_3D ( 'NONE', #6292, #7508, #3860 ) ;
#745 = CIRCLE ( 'NONE', #4086, 2.499999999999998668 ) ;
#746 = CARTESIAN_POINT ( 'NONE',  ( -4.101948962585905356, -2.368261337751088824, -3.681124513963624167 ) ) ;
#747 = CARTESIAN_POINT ( 'NONE',  ( -1.846868145590734756, -29.37500000136559564, -4.458734125000000326 ) ) ;
#748 = CIRCLE ( 'NONE', #8495, 5.000000000000000888 ) ;
#749 = FACE_OUTER_BOUND ( 'NONE', #2270, .T. ) ;
#750 = CARTESIAN_POINT ( 'NONE',  ( -2.390265326283148806, -4.391654775818394363, -4.375000000000000000 ) ) ;
#751 = ITEM_DEFINED_TRANSFORMATION ( 'NONE', 'NONE', #7349,  #3223 ) ;
#752 = CARTESIAN_POINT ( 'NONE',  ( 1.261996585732578113, -4.276409079477644148, -7.812499998634407916 ) ) ;
#753 = CARTESIAN_POINT ( 'NONE',  ( -3.753672977998669946, -3.033343224707661712, 1.365593156898739876E-09 ) ) ;
#754 = CIRCLE ( 'NONE', #9773, 4.999999999999997335 ) ;
#755 = ORIENTED_EDGE ( 'NONE', *, *, #9626, .F. ) ;
#756 = PRESENTATION_STYLE_ASSIGNMENT (( #11957 ) ) ;
#757 = VERTEX_POINT ( 'NONE', #7935 ) ;
#758 = CARTESIAN_POINT ( 'NONE',  ( 0.04606493828582666761, 9.175055303659577888, -8.057411785091799672 ) ) ;
#759 = VECTOR ( 'NONE', #12567, 1000.000000000000000 ) ;
#760 = ORIENTED_EDGE ( 'NONE', *, *, #7226, .T. ) ;
#761 = DIRECTION ( 'NONE',  ( 1.000000000000000000, 0.000000000000000000, 0.000000000000000000 ) ) ;
#762 = EDGE_CURVE ( 'NONE', #10581, #8118, #3944, .T. ) ;
#763 = ADVANCED_FACE ( 'NONE', ( #6395 ), #15112, .T. ) ;
#764 = DIRECTION ( 'NONE',  ( 0.000000000000000000, 0.000000000000000000, 1.000000000000000000 ) ) ;
#765 = DIRECTION ( 'NONE',  ( -0.000000000000000000, -0.000000000000000000, -1.000000000000000000 ) ) ;
#766 = CARTESIAN_POINT ( 'NONE',  ( -2.390265326283148806, -4.391654775818394363, -7.249999997268815832 ) ) ;
#767 = CARTESIAN_POINT ( 'NONE',  ( -3.401574460001765221, 4.209348295687701302, -0.6875000000000015543 ) ) ;
#768 = DIRECTION ( 'NONE',  ( 0.000000000000000000, 0.000000000000000000, 1.000000000000000000 ) ) ;
#769 = DIRECTION ( 'NONE',  ( 0.000000000000000000, 0.000000000000000000, 1.000000000000000000 ) ) ;
#770 = EDGE_LOOP ( 'NONE', ( #1058, #1735, #5015, #1295 ) ) ;
#771 = DIRECTION ( 'NONE',  ( 0.000000000000000000, 0.000000000000000000, 1.000000000000000000 ) ) ;
#772 = PLANE ( 'NONE',  #11770 ) ;
#773 = EDGE_LOOP ( 'NONE', ( #6443, #12124, #14926, #9073 ) ) ;
#774 = CARTESIAN_POINT ( 'NONE',  ( 5.000000000000000000, -27.00000000000000000, 0.000000000000000000 ) ) ;
#775 = ORIENTED_EDGE ( 'NONE', *, *, #5162, .T. ) ;
#776 = ORIENTED_EDGE ( 'NONE', *, *, #7729, .T. ) ;
#777 = CARTESIAN_POINT ( 'NONE',  ( 4.799145180956616130, -0.5093500532425063732, -0.6249999986344092484 ) ) ;
#778 = DIRECTION ( 'NONE',  ( 0.000000000000000000, 0.000000000000000000, 1.000000000000000000 ) ) ;
#779 = DIRECTION ( 'NONE',  ( 0.000000000000000000, -1.224646799147353454E-16, 1.000000000000000000 ) ) ;
#780 = EDGE_CURVE ( 'NONE', #7205, #11041, #8594, .T. ) ;
#781 = EDGE_CURVE ( 'NONE', #5812, #14017, #1873, .T. ) ;
#782 = LINE ( 'NONE', #14580, #15415 ) ;
#783 = FACE_BOUND ( 'NONE', #9056, .T. ) ;
#784 = CARTESIAN_POINT ( 'NONE',  ( -28.86751345948126257, 88.59290746114278647, -50.00000000000000711 ) ) ;
#785 = CARTESIAN_POINT ( 'NONE',  ( -114.9999999999999858, -115.2072594216369907, 17.50000000000000000 ) ) ;
#786 = PLANE ( 'NONE',  #13756 ) ;
#787 = CARTESIAN_POINT ( 'NONE',  ( 3.061616997868383141E-16, -24.87500000273118417, -5.000000000000000000 ) ) ;
#788 = CARTESIAN_POINT ( 'NONE',  ( 4.458734124999999437, -28.62500000136559564, -1.846868145590734978 ) ) ;
#789 =( BOUNDED_CURVE ( )  B_SPLINE_CURVE ( 2, ( #4267, #640, #11924, #7022, #15271, #3296, #14367, #4503, #1998 ),
 .UNSPECIFIED., .F., .F. ) 
 B_SPLINE_CURVE_WITH_KNOTS ( ( 3, 2, 2, 2, 3 ),
 ( 0.9545872658012772849, 0.9625000000000000222, 0.9749999999999999778, 0.9875000000000000444, 1.000000000000000000 ),
 .UNSPECIFIED. ) 
 CURVE ( )  GEOMETRIC_REPRESENTATION_ITEM ( )  RATIONAL_B_SPLINE_CURVE ( ( 0.9646335149384808183, 0.9518143178943441196, 1.000000000000000000, 0.9238795325112867385, 1.000000000000000000, 0.9238795325112867385, 1.000000000000000000, 0.9238795325112867385, 1.000000000000000000 ) ) 
 REPRESENTATION_ITEM ( '' )  );
#790 = SHAPE_REPRESENTATION ( 'socket head cap screw_iso_ISO 4762 M5 x 20 - 20N', ( #3223 ), #15084 ) ;
#791 = CARTESIAN_POINT ( 'NONE',  ( -3.753672977998669946, -3.033343224707661712, -1.749999998634408360 ) ) ;
#792 = ORIENTED_EDGE ( 'NONE', *, *, #4767, .T. ) ;
#793 = DIRECTION ( 'NONE',  ( 0.000000000000000000, 0.000000000000000000, 1.000000000000000000 ) ) ;
#794 = VERTEX_POINT ( 'NONE', #12509 ) ;
#795 = ORIENTED_EDGE ( 'NONE', *, *, #12841, .F. ) ;
#796 = CARTESIAN_POINT ( 'NONE',  ( 3.152801135295366208, -25.81250000136559564, 3.152801135295367985 ) ) ;
#797 = CARTESIAN_POINT ( 'NONE',  ( 31.75426480542940766, -37.00000000000000711, 15.00000000000001243 ) ) ;
#798 = DIRECTION ( 'NONE',  ( 0.4999999999999976685, 0.8660254037844399289, 0.000000000000000000 ) ) ;
#799 = EDGE_CURVE ( 'NONE', #3174, #2626, #1489, .T. ) ;
#800 = EDGE_CURVE ( 'NONE', #4542, #3229, #6635, .T. ) ;
#801 = CARTESIAN_POINT ( 'NONE',  ( 7.908230272949474227, -3.123266379892538858, -7.776722524729992259 ) ) ;
#802 = CARTESIAN_POINT ( 'NONE',  ( -3.916244202832140253, 2.131511515620587272, -6.937499998634407916 ) ) ;
#803 = CARTESIAN_POINT ( 'NONE',  ( 4.095339645587086963, -3.395032785697071009, 48.69265741069611408 ) ) ;
#804 = CARTESIAN_POINT ( 'NONE',  ( -3.535533905932738641, -26.37500000000000355, 3.535533905932737309 ) ) ;
#805 = CARTESIAN_POINT ( 'NONE',  ( 3.753672977998667726, 3.033343224707664376, -6.249999998634408804 ) ) ;
#806 = DIRECTION ( 'NONE',  ( -0.000000000000000000, -0.000000000000000000, 1.000000000000000000 ) ) ;
#807 = LINE ( 'NONE', #5727, #13340 ) ;
#808 = CARTESIAN_POINT ( 'NONE',  ( -3.152801135295367096, -29.06250000136559564, -3.152801135295367541 ) ) ;
#809 = ORIENTED_EDGE ( 'NONE', *, *, #11477, .T. ) ;
#810 = CARTESIAN_POINT ( 'NONE',  ( 4.458734124999999437, -24.43750000136559564, 0.000000000000000000 ) ) ;
#811 = DIRECTION ( 'NONE',  ( 1.319090325525611458E-16, 1.000000000000000000, 0.000000000000000000 ) ) ;
#812 = ORIENTED_EDGE ( 'NONE', *, *, #2570, .F. ) ;
#813 = ORIENTED_EDGE ( 'NONE', *, *, #12222, .F. ) ;
#814 = LINE ( 'NONE', #5734, #2541 ) ;
#815 = CARTESIAN_POINT ( 'NONE',  ( -3.152801135295367096, -28.06250000136559564, -3.152801135295367541 ) ) ;
#816 = CARTESIAN_POINT ( 'NONE',  ( -0.5711823568785977523, -5.381735091635034607, -7.187499997268816720 ) ) ;
#817 = EDGE_LOOP ( 'NONE', ( #5789, #2864, #13408 ) ) ;
#818 = CARTESIAN_POINT ( 'NONE',  ( -3.535533905932738641, -24.50000000273118772, 3.535533905932737309 ) ) ;
#819 = EDGE_CURVE ( 'NONE', #11041, #1955, #9872, .T. ) ;
#820 = CARTESIAN_POINT ( 'NONE',  ( -54.99999999999999289, -25.00000000000000000, 17.50000000000000000 ) ) ;
#821 = CARTESIAN_POINT ( 'NONE',  ( -3.152801135295367096, -26.31250000136559564, -3.152801135295367541 ) ) ;
#822 = DIRECTION ( 'NONE',  ( -1.000000000000000000, 0.000000000000000000, 1.239088197126290570E-16 ) ) ;
#823 = FACE_OUTER_BOUND ( 'NONE', #9623, .T. ) ;
#824 = PRESENTATION_STYLE_ASSIGNMENT (( #8512 ) ) ;
#825 = CARTESIAN_POINT ( 'NONE',  ( 0.000000000000000000, 37.00000000000000000, 0.000000000000000000 ) ) ;
#826 = AXIS2_PLACEMENT_3D ( 'NONE', #2213, #7167, #7316 ) ;
#827 = ORIENTED_EDGE ( 'NONE', *, *, #12141, .F. ) ;
#828 =( NAMED_UNIT ( * ) PLANE_ANGLE_UNIT ( ) SI_UNIT ( $, .RADIAN. ) );
#829 = EDGE_LOOP ( 'NONE', ( #13631, #3584, #12937, #6136 ) ) ;
#830 = CARTESIAN_POINT ( 'NONE',  ( -1.015826369458357803, 8.073766409984798997, -7.642786413620218156 ) ) ;
#831 = ORIENTED_EDGE ( 'NONE', *, *, #10965, .F. ) ;
#832 =( REPRESENTATION_RELATIONSHIP ('NONE','NONE', #4176, #4696 ) REPRESENTATION_RELATIONSHIP_WITH_TRANSFORMATION ( #5278 )SHAPE_REPRESENTATION_RELATIONSHIP( ) );
#833 = ADVANCED_FACE ( 'NONE', ( #10189, #4033, #2825, #6724, #1611 ), #415, .T. ) ;
#834 = DIRECTION ( 'NONE',  ( 0.000000000000000000, -1.000000000000000000, 1.287488025362403787E-15 ) ) ;
#835 = CARTESIAN_POINT ( 'NONE',  ( -39.99999999999999289, -11.00000000000000178, 2.500000000001739497 ) ) ;
#836 = CARTESIAN_POINT ( 'NONE',  ( 3.061616997868383141E-16, -27.75000000000000000, -5.000000000000000000 ) ) ;
#837 = DIRECTION ( 'NONE',  ( 1.000000000000000000, -6.123233995736766036E-17, -6.123233995736764803E-17 ) ) ;
#838 = CARTESIAN_POINT ( 'NONE',  ( -4.795541693661363958, -1.415196051561583790, -7.374999997268815832 ) ) ;
#839 = LINE ( 'NONE', #5761, #4644 ) ;
#840 = CARTESIAN_POINT ( 'NONE',  ( 11.91154273188014301, -5.000000000000000000, -56.63139720814413636 ) ) ;
#841 = DIRECTION ( 'NONE',  ( 0.000000000000000000, 0.000000000000000000, 1.000000000000000000 ) ) ;
#842 = ORIENTED_EDGE ( 'NONE', *, *, #8606, .F. ) ;
#843 = DIRECTION ( 'NONE',  ( -1.000000000000000000, -0.000000000000000000, -0.000000000000000000 ) ) ;
#844 = DIRECTION ( 'NONE',  ( 0.000000000000000000, 0.000000000000000000, -1.000000000000000000 ) ) ;
#845 = LINE ( 'NONE', #15641, #3770 ) ;
#846 = EDGE_CURVE ( 'NONE', #8138, #15819, #13214, .T. ) ;
#847 = EDGE_LOOP ( 'NONE', ( #5663, #1091, #13175, #4409, #14855 ) ) ;
#848 = DIRECTION ( 'NONE',  ( 0.000000000000000000, 0.000000000000000000, 1.000000000000000000 ) ) ;
#849 = ORIENTED_EDGE ( 'NONE', *, *, #13885, .T. ) ;
#850 = AXIS2_PLACEMENT_3D ( 'NONE', #4119, #1694, #1775 ) ;
#851 = EDGE_LOOP ( 'NONE', ( #9621, #3536, #2832, #14469 ) ) ;
#852 = FACE_OUTER_BOUND ( 'NONE', #5733, .T. ) ;
#853 = DIRECTION ( 'NONE',  ( 0.000000000000000000, 1.000000000000000000, 0.000000000000000000 ) ) ;
#854 = CIRCLE ( 'NONE', #9367, 2.499999999999998668 ) ;
#855 = DIRECTION ( 'NONE',  ( -0.8660254037844387076, -0.000000000000000000, -0.5000000000000003331 ) ) ;
#856 = LINE ( 'NONE', #14435, #15169 ) ;
#857 = CARTESIAN_POINT ( 'NONE',  ( 4.769696007084728073, -20.00000000000000000, -1.500000000000000000 ) ) ;
#858 = CYLINDRICAL_SURFACE ( 'NONE', #8255, 5.000000000000000000 ) ;
#859 = CARTESIAN_POINT ( 'NONE',  ( -2.390265326283148806, -4.391654775818394363, -7.375000000000002665 ) ) ;
#860 = DIRECTION ( 'NONE',  ( -1.000000000000000000, 0.000000000000000000, 0.000000000000000000 ) ) ;
#861 = B_SPLINE_CURVE_WITH_KNOTS ( 'NONE', 3,
 ( #8485, #2391, #13222, #14609, #9530, #8331, #9837, #7427, #1269, #12332, #13384, #7266, #6214, #11129, #2160, #7340, #3380, #7109, #14533, #10821, #14459, #12245, #12012, #5888, #15761, #12167, #2233, #4911, #9671, #1186, #4672, #7194, #6131, #1034 ),
 .UNSPECIFIED., .F., .F.,
 ( 4, 2, 2, 2, 2, 2, 2, 2, 2, 2, 2, 2, 2, 2, 2, 2, 4 ),
 ( 0.007748559620023459139, 0.008546605054884921782, 0.009344650489746383556, 0.01014269592460784707, 0.01094074135946930884, 0.01173878679433077235, 0.01253683222919223586, 0.01333487766405369590, 0.01413292309891515941, 0.01493096853377662292, 0.01572901396863808643, 0.01652705940349954994, 0.01732510483836101345, 0.01812315027322247696, 0.01892119570808394047, 0.01971924114294540398, 0.02051728657780686749 ),
 .UNSPECIFIED. ) ;
#862 = FILL_AREA_STYLE_COLOUR ( '', #3052 ) ;
#863 = CARTESIAN_POINT ( 'NONE',  ( 1.846868145590736310, -27.87500000136559564, 4.458734124999997661 ) ) ;
#864 = CARTESIAN_POINT ( 'NONE',  ( 3.916244202832140253, -2.131511515620588160, -0.4374999986344086933 ) ) ;
#865 = VERTEX_POINT ( 'NONE', #5510 ) ;
#866 = DIRECTION ( 'NONE',  ( 1.000000000000000000, -0.000000000000000000, 1.114413700119375779E-16 ) ) ;
#867 = EDGE_CURVE ( 'NONE', #14345, #10556, #6652, .T. ) ;
#868 = ORIENTED_EDGE ( 'NONE', *, *, #15692, .F. ) ;
#869 = VERTEX_POINT ( 'NONE', #9235 ) ;
#870 = ADVANCED_FACE ( 'NONE', ( #1789 ), #9154, .T. ) ;
#871 = SURFACE_STYLE_USAGE ( .BOTH. , #2225 ) ;
#872 = ORIENTED_EDGE ( 'NONE', *, *, #6146, .F. ) ;
#873 = PRODUCT ( 'hex flange nut gradea_iso_ISO - 4161 - M5 - N', 'hex flange nut gradea_iso_ISO - 4161 - M5 - N', '', ( #14449 ) ) ;
#874 = VECTOR ( 'NONE', #4573, 1000.000000000000000 ) ;
#875 = CARTESIAN_POINT ( 'NONE',  ( 1.846868145590735200, -25.50000000136559919, -4.458734125000000326 ) ) ;
#876 = CARTESIAN_POINT ( 'NONE',  ( -3.861362476283256129, -2.629030857716004199, -3.671615880910374941 ) ) ;
#877 = CARTESIAN_POINT ( 'NONE',  ( 7.922281120364393914, 4.573931137438269623, -8.047472243342932430 ) ) ;
#878 = CARTESIAN_POINT ( 'NONE',  ( -3.033343224707664820, 3.753672977998667726, -4.999999998634407028 ) ) ;
#879 = PLANE ( 'NONE',  #593 ) ;
#880 =( BOUNDED_CURVE ( )  B_SPLINE_CURVE ( 2, ( #1973, #6919, #693, #11825, #774, #5696, #10633, #15564, #1149 ),
 .UNSPECIFIED., .F., .F. ) 
 B_SPLINE_CURVE_WITH_KNOTS ( ( 3, 2, 2, 2, 3 ),
 ( 0.4750000000000000888, 0.4875000000000000999, 0.5000000000000001110, 0.5125000000000000666, 0.5250000000000001332 ),
 .UNSPECIFIED. ) 
 CURVE ( )  GEOMETRIC_REPRESENTATION_ITEM ( )  RATIONAL_B_SPLINE_CURVE ( ( 0.9999999999999993339, 0.9238795325112874046, 1.000000000000000000, 0.9238795325112867385, 1.000000000000000000, 0.9238795325112867385, 1.000000000000000000, 0.9238795325112860723, 1.000000000000000666 ) ) 
 REPRESENTATION_ITEM ( '' )  );
#881 = DIRECTION ( 'NONE',  ( -0.000000000000000000, -1.000000000000000000, -0.000000000000000000 ) ) ;
#882 = CARTESIAN_POINT ( 'NONE',  ( 4.795541693661363958, 1.415196051561583790, 0.9999999999999974465 ) ) ;
#883 = CARTESIAN_POINT ( 'NONE',  ( -39.99999999999999289, -11.00000000000000178, -2.500000000000079492 ) ) ;
#884 = DIRECTION ( 'NONE',  ( 0.000000000000000000, 0.000000000000000000, -1.000000000000000000 ) ) ;
#885 = CARTESIAN_POINT ( 'NONE',  ( 1.846868145590736310, -29.62500000136559208, 4.458734124999999437 ) ) ;
#886 = ORIENTED_EDGE ( 'NONE', *, *, #12520, .T. ) ;
#887 = CARTESIAN_POINT ( 'NONE',  ( -1.846868145590737420, -23.75000000136559564, 4.458734124999997661 ) ) ;
#888 = EDGE_CURVE ( 'NONE', #7896, #6707, #587, .T. ) ;
#889 = PLANE ( 'NONE',  #14594 ) ;
#890 = ORIENTED_EDGE ( 'NONE', *, *, #4257, .T. ) ;
#891 = EDGE_LOOP ( 'NONE', ( #10651, #6417, #11764, #201 ) ) ;
#892 = EDGE_CURVE ( 'NONE', #13370, #11577, #1632, .T. ) ;
#893 = CARTESIAN_POINT ( 'NONE',  ( -3.999999999999999112, 1.539600717838996324, -3.300726591567078039 ) ) ;
#894 = COLOUR_RGB ( '', 0.40784314, 0.44705882, 0.49803922) ;
#895 = CARTESIAN_POINT ( 'NONE',  ( -4.458734124999999437, -29.93750000136559564, -5.460374474430324690E-16 ) ) ;
#896 = PLANE ( 'NONE',  #9190 ) ;
#897 = ORIENTED_EDGE ( 'NONE', *, *, #7225, .T. ) ;
#898 = CARTESIAN_POINT ( 'NONE',  ( -5.000000000000000888, -24.56250000273118772, 2.071067811865474617 ) ) ;
#899 = FACE_OUTER_BOUND ( 'NONE', #14701, .T. ) ;
#900 = CARTESIAN_POINT ( 'NONE',  ( 40.53271815135278899, -3.097286126993895827, -27.46394321569970742 ) ) ;
#901 = CARTESIAN_POINT ( 'NONE',  ( -8.190561711645485556E-16, -28.93750000136559564, 4.458734124999999437 ) ) ;
#902 = DIRECTION ( 'NONE',  ( 0.000000000000000000, 0.000000000000000000, 1.000000000000000000 ) ) ;
#903 = CARTESIAN_POINT ( 'NONE',  ( -5.000000000000002665, 1.292545281756915047E-15, -0.4202630448617610814 ) ) ;
#904 = CARTESIAN_POINT ( 'NONE',  ( 0.000000000000000000, -1.178949249685213863, 2.042000000000002924 ) ) ;
#905 = EDGE_CURVE ( 'NONE', #560, #1675, #15053, .T. ) ;
#907 = EDGE_CURVE ( 'NONE', #8217, #4663, #4887, .T. ) ;
#906 = ORIENTED_EDGE ( 'NONE', *, *, #15328, .F. ) ;
#908 = EDGE_CURVE ( 'NONE', #2200, #11431, #10878, .T. ) ;
#909 = ORIENTED_EDGE ( 'NONE', *, *, #7781, .F. ) ;
#910 = FACE_OUTER_BOUND ( 'NONE', #9958, .T. ) ;
#911 =( GEOMETRIC_REPRESENTATION_CONTEXT ( 3 ) GLOBAL_UNCERTAINTY_ASSIGNED_CONTEXT ( ( #10140 ) ) GLOBAL_UNIT_ASSIGNED_CONTEXT ( ( #15799, #6830, #4795 ) ) REPRESENTATION_CONTEXT ( 'NONE', 'WORKASPACE' ) );
#912 = ORIENTED_EDGE ( 'NONE', *, *, #2834, .T. ) ;
#913 = VECTOR ( 'NONE', #15309, 1000.000000000000114 ) ;
#914 = CYLINDRICAL_SURFACE ( 'NONE', #5036, 2.500000000000909495 ) ;
#915 = CARTESIAN_POINT ( 'NONE',  ( -4.209348295687703079, -3.401574460001763445, -3.312499997268815832 ) ) ;
#916 = CARTESIAN_POINT ( 'NONE',  ( -0.5093500532425060401, -4.799145180956616130, -0.6249999986344055847 ) ) ;
#917 = CARTESIAN_POINT ( 'NONE',  ( 0.000000000000000000, 0.000000000000000000, 0.000000000000000000 ) ) ;
#918 = AXIS2_PLACEMENT_3D ( 'NONE', #15837, #15765, #9600 ) ;
#919 = CARTESIAN_POINT ( 'NONE',  ( 3.753672977998667726, 3.033343224707664376, -1.499999998634408138 ) ) ;
#920 =( NAMED_UNIT ( * ) SI_UNIT ( $, .STERADIAN. ) SOLID_ANGLE_UNIT ( ) );
#921 = CARTESIAN_POINT ( 'NONE',  ( -67.50000000000000000, 40.00000000000000000, 2.649999999999285816 ) ) ;
#922 = ORIENTED_EDGE ( 'NONE', *, *, #9390, .F. ) ;
#923 = CIRCLE ( 'NONE', #10224, 39.99999999999999289 ) ;
#924 = PLANE ( 'NONE',  #8231 ) ;
#925 = EDGE_CURVE ( 'NONE', #3643, #15644, #11415, .T. ) ;
#926 = AXIS2_PLACEMENT_3D ( 'NONE', #14707, #3629, #488 ) ;
#927 = CONTEXT_DEPENDENT_SHAPE_REPRESENTATION ( #8886, #1456 ) ;
#928 = VERTEX_POINT ( 'NONE', #6734 ) ;
#929 = CARTESIAN_POINT ( 'NONE',  ( 6.000000000000000000, -13.00000000000000178, 1.500000000000000000 ) ) ;
#930 = ORIENTED_EDGE ( 'NONE', *, *, #7501, .T. ) ;
#931 = ORIENTED_EDGE ( 'NONE', *, *, #3922, .F. ) ;
#932 = FACE_OUTER_BOUND ( 'NONE', #10497, .T. ) ;
#933 = CIRCLE ( 'NONE', #2729, 5.000000000000000000 ) ;
#934 = EDGE_CURVE ( 'NONE', #2513, #13261, #602, .T. ) ;
#935 = CARTESIAN_POINT ( 'NONE',  ( 0.000000000000000000, -20.00000000000000000, 0.000000000000000000 ) ) ;
#936 = DIRECTION ( 'NONE',  ( 0.000000000000000000, 0.000000000000000000, -1.000000000000000000 ) ) ;
#937 = CARTESIAN_POINT ( 'NONE',  ( 0.5711823568785989735, 5.381735091635026613, -0.6874999972688189409 ) ) ;
#938 = LINE ( 'NONE', #7086, #874 ) ;
#939 = AXIS2_PLACEMENT_3D ( 'NONE', #4303, #9243, #3246 ) ;
#940 = CARTESIAN_POINT ( 'NONE',  ( -8.190561711645485556E-16, -30.93750000136559564, 4.458734124999999437 ) ) ;
#941 = CARTESIAN_POINT ( 'NONE',  ( -1.261996585732579224, 4.276409079477648589, 0.9375000013655925279 ) ) ;
#942 = ORIENTED_EDGE ( 'NONE', *, *, #5179, .F. ) ;
#943 = AXIS2_PLACEMENT_3D ( 'NONE', #9492, #14262, #5694 ) ;
#944 = CARTESIAN_POINT ( 'NONE',  ( 1.060314165523342567, 8.048081368954365544, -7.659344964962869540 ) ) ;
#945 = EDGE_LOOP ( 'NONE', ( #10035, #9827 ) ) ;
#946 = VERTEX_POINT ( 'NONE', #1706 ) ;
#947 = CIRCLE ( 'NONE', #5073, 2.649999999999992806 ) ;
#948 = ORIENTED_EDGE ( 'NONE', *, *, #3086, .T. ) ;
#949 = AXIS2_PLACEMENT_3D ( 'NONE', #12692, #12456, #11172 ) ;
#950 = CARTESIAN_POINT ( 'NONE',  ( -8.190561711645485556E-16, -26.93750000136559564, 4.458734124999999437 ) ) ;
#951 = DIRECTION ( 'NONE',  ( 0.000000000000000000, 0.000000000000000000, 1.000000000000000000 ) ) ;
#952 = DIRECTION ( 'NONE',  ( 0.000000000000000000, 1.000000000000000000, 0.000000000000000000 ) ) ;
#953 = EDGE_CURVE ( 'NONE', #7835, #12023, #11561, .T. ) ;
#954 = CARTESIAN_POINT ( 'NONE',  ( -28.86751345948129455, -37.00000000000000711, 49.99999999999999289 ) ) ;
#955 = CARTESIAN_POINT ( 'NONE',  ( 1.734723475976807094E-15, 4.618802153517012954, -0.4999999999999995559 ) ) ;
#956 = ADVANCED_FACE ( 'NONE', ( #10366 ), #15296, .F. ) ;
#957 = AXIS2_PLACEMENT_3D ( 'NONE', #1552, #8835, #10207 ) ;
#958 = AXIS2_PLACEMENT_3D ( 'NONE', #7043, #8272, #6887 ) ;
#959 = CARTESIAN_POINT ( 'NONE',  ( 5.000000000000000000, -23.06250000000000000, 2.071067811865478614 ) ) ;
#960 = CARTESIAN_POINT ( 'NONE',  ( 0.5711823568785989735, 5.381735091635026613, -1.812500000000000888 ) ) ;
#961 = CARTESIAN_POINT ( 'NONE',  ( -5.000000000000000000, -21.62500000273118772, -6.123233995736766282E-16 ) ) ;
#962 = CARTESIAN_POINT ( 'NONE',  ( 3.061616997868383141E-16, -27.75000000000000000, -5.000000000000000000 ) ) ;
#963 = CARTESIAN_POINT ( 'NONE',  ( -9.184850993605147944E-16, -22.37500000273118417, 5.000000000000000000 ) ) ;
#964 = ORIENTED_EDGE ( 'NONE', *, *, #14576, .F. ) ;
#965 = CARTESIAN_POINT ( 'NONE',  ( 0.000000000000000000, 0.000000000000000000, 0.000000000000000000 ) ) ;
#966 = ORIENTED_EDGE ( 'NONE', *, *, #12050, .T. ) ;
#967 = AXIS2_PLACEMENT_3D ( 'NONE', #14438, #8069, #12965 ) ;
#968 = EDGE_LOOP ( 'NONE', ( #5323, #8194, #3762, #2718 ) ) ;
#969 = CARTESIAN_POINT ( 'NONE',  ( -7.500000000000003553, -0.7583608255762881445, -7.446489218764575035 ) ) ;
#970 = CARTESIAN_POINT ( 'NONE',  ( -8.190561711645485556E-16, -28.68750000136559564, 4.458734124999999437 ) ) ;
#971 = FACE_OUTER_BOUND ( 'NONE', #5873, .T. ) ;
#972 = ORIENTED_EDGE ( 'NONE', *, *, #6643, .F. ) ;
#973 = CARTESIAN_POINT ( 'NONE',  ( -2.071067811865492381, -24.43750000273118772, 4.999999999999985789 ) ) ;
#974 =( BOUNDED_CURVE ( )  B_SPLINE_CURVE ( 2, ( #5596, #5515, #12932, #4387, #6567 ),
 .UNSPECIFIED., .F., .F. ) 
 B_SPLINE_CURVE_WITH_KNOTS ( ( 3, 2, 3 ),
 ( 0.000000000000000000, 0.01250000000000001110, 0.02500000000000002220 ),
 .UNSPECIFIED. ) 
 CURVE ( )  GEOMETRIC_REPRESENTATION_ITEM ( )  RATIONAL_B_SPLINE_CURVE ( ( 1.000000000000000000, 0.9238795325112867385, 1.000000000000000000, 0.9238795325112866275, 1.000000000000000222 ) ) 
 REPRESENTATION_ITEM ( '' )  );
#976 = AXIS2_PLACEMENT_3D ( 'NONE', #15540, #4455, #14550 ) ;
#975 = DIRECTION ( 'NONE',  ( -0.000000000000000000, -1.000000000000000000, -0.000000000000000000 ) ) ;
#977 = DIRECTION ( 'NONE',  ( -0.8660254037844401509, 0.4999999999999973355, -0.000000000000000000 ) ) ;
#978 = CARTESIAN_POINT ( 'NONE',  ( 40.62171971187174790, -3.060691311048529872, -27.36941859593484949 ) ) ;
#979 = EDGE_CURVE ( 'NONE', #13100, #8026, #12847, .T. ) ;
#980 = CARTESIAN_POINT ( 'NONE',  ( -1.846868145590734756, -23.37500000136559564, -4.458734125000000326 ) ) ;
#981 = CARTESIAN_POINT ( 'NONE',  ( 3.540020015735602765, 2.810662092924382627, -3.602146406945867962 ) ) ;
#982 = CARTESIAN_POINT ( 'NONE',  ( 0.6666666666666689611, 4.233901974057261874, -3.300726591567082480 ) ) ;
#983 = CARTESIAN_POINT ( 'NONE',  ( -2.071067811865475061, -30.81250000273118772, -5.000000000000000888 ) ) ;
#984 = CARTESIAN_POINT ( 'NONE',  ( 4.896370289182470081, -5.000000000000000000, -48.48076211353470910 ) ) ;
#985 = ORIENTED_EDGE ( 'NONE', *, *, #11874, .T. ) ;
#986 = AXIS2_PLACEMENT_3D ( 'NONE', #11840, #10645, #6771 ) ;
#987 = ORIENTED_EDGE ( 'NONE', *, *, #14160, .T. ) ;
#988 = MECHANICAL_DESIGN_GEOMETRIC_PRESENTATION_REPRESENTATION (  '', ( #3323 ), #4608 ) ;
#989 = ORIENTED_EDGE ( 'NONE', *, *, #8609, .T. ) ;
#990 = AXIS2_PLACEMENT_3D ( 'NONE', #10557, #15485, #3024 ) ;
#991 = EDGE_CURVE ( 'NONE', #3918, #7223, #6486, .T. ) ;
#992 = ADVANCED_FACE ( 'NONE', ( #2100 ), #5909, .T. ) ;
#993 = CARTESIAN_POINT ( 'NONE',  ( 3.753672977998667726, 3.033343224707664376, -1.249999998634407916 ) ) ;
#994 = VECTOR ( 'NONE', #10000, 1000.000000000000000 ) ;
#995 = DIRECTION ( 'NONE',  ( 0.000000000000000000, 0.000000000000000000, 1.000000000000000000 ) ) ;
#996 = CARTESIAN_POINT ( 'NONE',  ( 1.261996585732578113, -4.276409079477644148, -0.8124999986344090264 ) ) ;
#997 = DIRECTION ( 'NONE',  ( 0.000000000000000000, -1.224646799147353454E-16, 1.000000000000000000 ) ) ;
#998 = CARTESIAN_POINT ( 'NONE',  ( 3.510273485745307731, 2.827716139362654424, -3.610536846335885564 ) ) ;
#999 = ORIENTED_EDGE ( 'NONE', *, *, #10649, .T. ) ;
#1000 = DIRECTION ( 'NONE',  ( -0.000000000000000000, -1.000000000000000000, -0.000000000000000000 ) ) ;
#1001 = B_SPLINE_CURVE_WITH_KNOTS ( 'NONE', 3,
 ( #3864, #8803, #1524, #1431, #8726, #6461 ),
 .UNSPECIFIED., .F., .F.,
 ( 4, 2, 4 ),
 ( 0.000000000000000000, 0.002307655110370376069, 0.004615310220740751271 ),
 .UNSPECIFIED. ) ;
#1002 = AXIS2_PLACEMENT_3D ( 'NONE', #8932, #7733, #12625 ) ;
#1003 = CARTESIAN_POINT ( 'NONE',  ( 35.00000000000000000, 50.00000000000000000, 2.649999999999985700 ) ) ;
#1004 = ORIENTED_EDGE ( 'NONE', *, *, #13938, .T. ) ;
#1005 = CYLINDRICAL_SURFACE ( 'NONE', #2041, 2.499999999999998668 ) ;
#1006 = EDGE_LOOP ( 'NONE', ( #7439, #10537, #3336, #10117, #9918, #9746, #14886, #3496 ) ) ;
#1007 = ORIENTED_EDGE ( 'NONE', *, *, #15616, .T. ) ;
#1008 = CARTESIAN_POINT ( 'NONE',  ( -3.916244202832140253, 2.131511515620587272, -1.187499998634405918 ) ) ;
#1009 = AXIS2_PLACEMENT_3D ( 'NONE', #9184, #7818, #10391 ) ;
#1010 = CARTESIAN_POINT ( 'NONE',  ( -19.99999999999956657, -11.00000000000000178, 8.786575603324269439E-13 ) ) ;
#1011 = EDGE_CURVE ( 'NONE', #9125, #9091, #1099, .T. ) ;
#1012 = DIRECTION ( 'NONE',  ( 0.000000000000000000, 0.000000000000000000, 1.000000000000000000 ) ) ;
#1013 = CARTESIAN_POINT ( 'NONE',  ( -150.5560796608385203, -71.58493649053926333, -17.50000000000000000 ) ) ;
#1014 = LINE ( 'NONE', #9427, #7731 ) ;
#1015 = CARTESIAN_POINT ( 'NONE',  ( 4.795541693661363958, 1.415196051561583790, 0.1250000027311834461 ) ) ;
#1016 = LINE ( 'NONE', #4965, #2526 ) ;
#1017 = DIRECTION ( 'NONE',  ( 0.000000000000000000, 1.000000000000000000, 0.000000000000000000 ) ) ;
#1018 = CARTESIAN_POINT ( 'NONE',  ( -3.152801135295367985, -29.06250000136559564, 3.152801135295367096 ) ) ;
#1019 = CARTESIAN_POINT ( 'NONE',  ( 4.799145180956616130, -0.5093500532425063732, -4.374999998634405252 ) ) ;
#1020 = ORIENTED_EDGE ( 'NONE', *, *, #12841, .T. ) ;
#1021 = AXIS2_PLACEMENT_3D ( 'NONE', #527, #286, #7723 ) ;
#1022 = CARTESIAN_POINT ( 'NONE',  ( 16.49999999999956657, -8.786575603324269439E-13, 1.500000000000000000 ) ) ;
#1023 = ORIENTED_EDGE ( 'NONE', *, *, #8305, .F. ) ;
#1024 = ORIENTED_EDGE ( 'NONE', *, *, #7059, .T. ) ;
#1025 = ORIENTED_EDGE ( 'NONE', *, *, #5189, .F. ) ;
#1026 = CARTESIAN_POINT ( 'NONE',  ( -1.846868145590734756, -23.37500000136559564, -4.458734125000000326 ) ) ;
#1027 = CARTESIAN_POINT ( 'NONE',  ( -35.00000000000000000, 37.00000000000000000, 0.000000000000000000 ) ) ;
#1028 = FACE_BOUND ( 'NONE', #13834, .T. ) ;
#1029 = FACE_BOUND ( 'NONE', #10956, .T. ) ;
#1030 = CARTESIAN_POINT ( 'NONE',  ( 19.99999999999956657, -8.786575603324269439E-13, 1.500000000000000000 ) ) ;
#1031 = DIRECTION ( 'NONE',  ( 0.000000000000000000, 0.000000000000000000, -1.000000000000000000 ) ) ;
#1032 = CARTESIAN_POINT ( 'NONE',  ( 0.5711823568785989735, 5.381735091635026613, 0.1874999999999973355 ) ) ;
#1033 = DIRECTION ( 'NONE',  ( 0.000000000000000000, 0.000000000000000000, 1.000000000000000000 ) ) ;
#1034 = CARTESIAN_POINT ( 'NONE',  ( 4.391654732552941809, -2.390265405775130692, 0.000000000000000000 ) ) ;
#1035 = CARTESIAN_POINT ( 'NONE',  ( 5.000000000000000888, -22.06250000273119127, -2.071067811865475505 ) ) ;
#1036 = CARTESIAN_POINT ( 'NONE',  ( -3.916244202832140253, 2.131511515620587272, 0.8125000013655924169 ) ) ;
#1037 = VERTEX_POINT ( 'NONE', #9465 ) ;
#1038 = DIRECTION ( 'NONE',  ( 0.000000000000000000, 1.000000000000000000, 0.000000000000000000 ) ) ;
#1039 = ORIENTED_EDGE ( 'NONE', *, *, #7878, .T. ) ;
#1040 = EDGE_LOOP ( 'NONE', ( #12922, #2165, #8177, #15346 ) ) ;
#1041 = CARTESIAN_POINT ( 'NONE',  ( -7.500000000000002665, 1.613867362005931172, -7.450195926347909392 ) ) ;
#1042 = CARTESIAN_POINT ( 'NONE',  ( -3.152801135295367096, -29.06250000136559564, -3.152801135295367541 ) ) ;
#1043 = EDGE_CURVE ( 'NONE', #8138, #8374, #4686, .T. ) ;
#1044 = LINE ( 'NONE', #14705, #13288 ) ;
#1045 = ORIENTED_EDGE ( 'NONE', *, *, #12820, .F. ) ;
#1046 = DIRECTION ( 'NONE',  ( 0.9999824063907751803, 0.005931855436079011210, -0.000000000000000000 ) ) ;
#1047 = CARTESIAN_POINT ( 'NONE',  ( 6.000000000000000000, -20.00000000000000000, 1.500000000000000000 ) ) ;
#1048 = FACE_OUTER_BOUND ( 'NONE', #5833, .T. ) ;
#1049 = CARTESIAN_POINT ( 'NONE',  ( 2.500000000000000000, -1.178949249685213863, 2.042000000000002924 ) ) ;
#1050 = CARTESIAN_POINT ( 'NONE',  ( -1.846868145590734756, -22.37500000136559564, -4.458734125000000326 ) ) ;
#1051 = LINE ( 'NONE', #12031, #10121 ) ;
#1052 = CARTESIAN_POINT ( 'NONE',  ( 5.000000000000004441, 3.034671531081452754E-15, -0.9202630448617579173 ) ) ;
#1053 = CARTESIAN_POINT ( 'NONE',  ( -5.000000000000000888, -30.68750000273118772, -2.071067811865475949 ) ) ;
#1054 = CARTESIAN_POINT ( 'NONE',  ( -0.5711823568785977523, -5.381735091635034607, -6.187499997268815832 ) ) ;
#1055 = FACE_OUTER_BOUND ( 'NONE', #5659, .T. ) ;
#1056 = ORIENTED_EDGE ( 'NONE', *, *, #14475, .T. ) ;
#1058 = ORIENTED_EDGE ( 'NONE', *, *, #12944, .T. ) ;
#1057 = EDGE_CURVE ( 'NONE', #5664, #15429, #10141, .T. ) ;
#1059 = CARTESIAN_POINT ( 'NONE',  ( 2.500000000000000000, 2.357898499370433054, -1.951563910473907981E-15 ) ) ;
#1060 = EDGE_CURVE ( 'NONE', #5100, #14039, #4611, .T. ) ;
#1061 =( BOUNDED_CURVE ( )  B_SPLINE_CURVE ( 2, ( #5618, #15561, #3267, #4404, #15486, #8214, #11896, #9412, #14340, #13113, #10702 ),
 .UNSPECIFIED., .F., .F. ) 
 B_SPLINE_CURVE_WITH_KNOTS ( ( 3, 2, 2, 2, 2, 3 ),
 ( 0.3545872658012772516, 0.3624999999999999889, 0.3750000000000000000, 0.3875000000000000111, 0.4000000000000000222, 0.4045872658012772960 ),
 .UNSPECIFIED. ) 
 CURVE ( )  GEOMETRIC_REPRESENTATION_ITEM ( )  RATIONAL_B_SPLINE_CURVE ( ( 0.9646335149384808183, 0.9518143178943437865, 1.000000000000000000, 0.9238795325112867385, 1.000000000000000000, 0.9238795325112867385, 1.000000000000000000, 0.9238795325112867385, 1.000000000000000000, 0.9720652146169428409, 0.9646335149384805963 ) ) 
 REPRESENTATION_ITEM ( '' )  );
#1062 = ORIENTED_EDGE ( 'NONE', *, *, #11599, .T. ) ;
#1063 = DIRECTION ( 'NONE',  ( 0.000000000000000000, -1.287488025362403787E-15, -1.000000000000000000 ) ) ;
#1064 = PLANE ( 'NONE',  #10813 ) ;
#1065 = CARTESIAN_POINT ( 'NONE',  ( 2.131511515620586383, 3.916244202832140253, -1.187499998634405918 ) ) ;
#1066 = CARTESIAN_POINT ( 'NONE',  ( 42.02221399786068901, 6.999999999999999112, 1.053699678052475622E-13 ) ) ;
#1067 = CARTESIAN_POINT ( 'NONE',  ( 0.5093500532425063732, 4.799145180956616130, -2.374999998634407028 ) ) ;
#1068 =( NAMED_UNIT ( * ) PLANE_ANGLE_UNIT ( ) SI_UNIT ( $, .RADIAN. ) );
#1069 = EDGE_LOOP ( 'NONE', ( #13580, #15469, #3315, #3056 ) ) ;
#1070 = CARTESIAN_POINT ( 'NONE',  ( -1.154700538379255903, 0.000000000000000000, 34.00000000000000000 ) ) ;
#1071 =( LENGTH_UNIT ( ) NAMED_UNIT ( * ) SI_UNIT ( .MILLI., .METRE. ) );
#1072 = EDGE_CURVE ( 'NONE', #12769, #13901, #14197, .T. ) ;
#1073 = ORIENTED_EDGE ( 'NONE', *, *, #9578, .F. ) ;
#1074 = CARTESIAN_POINT ( 'NONE',  ( 4.204115023516791005, -1.660442669500199919, -3.602151381774560068 ) ) ;
#1075 = CARTESIAN_POINT ( 'NONE',  ( 42.02221399786069611, -1.230770033143087371E-15, -2.649999999999878231 ) ) ;
#1076 = ADVANCED_FACE ( 'NONE', ( #7046 ), #10609, .T. ) ;
#1077 = ORIENTED_EDGE ( 'NONE', *, *, #6645, .T. ) ;
#1078 = CARTESIAN_POINT ( 'NONE',  ( 3.033343224707661712, -3.753672977998669502, -4.749999998634407028 ) ) ;
#1079 = CONICAL_SURFACE ( 'NONE', #5723, 4.174999999999999822, 0.9599310885968795892 ) ;
#1080 = SURFACE_SIDE_STYLE ('',( #10941 ) ) ;
#1081 = CARTESIAN_POINT ( 'NONE',  ( -3.753672977998669502, -3.033343224707661712, -7.749999998634409692 ) ) ;
#1082 = LINE ( 'NONE', #14504, #5613 ) ;
#1083 = CARTESIAN_POINT ( 'NONE',  ( -111.3391301858327296, -111.5473609024183475, 17.50000000000000000 ) ) ;
#1084 = LINE ( 'NONE', #9647, #11321 ) ;
#1085 = CARTESIAN_POINT ( 'NONE',  ( 2.484690871711851132E-16, -8.716842316802402735, -7.700127545397319473 ) ) ;
#1086 = CARTESIAN_POINT ( 'NONE',  ( -5.000000000000000000, -24.50000000000000000, -6.123233995736766282E-16 ) ) ;
#1087 = SURFACE_SIDE_STYLE ('',( #12150 ) ) ;
#1088 = CARTESIAN_POINT ( 'NONE',  ( 3.152801135295367541, -26.56250000136559564, -3.152801135295367541 ) ) ;
#1089 = CARTESIAN_POINT ( 'NONE',  ( -4.276409079477644148, -1.261996585732578335, -3.812499998634404808 ) ) ;
#1090 = CYLINDRICAL_SURFACE ( 'NONE', #14091, 10.00000000000000000 ) ;
#1091 = ORIENTED_EDGE ( 'NONE', *, *, #10222, .T. ) ;
#1092 = VECTOR ( 'NONE', #10245, 1000.000000000000000 ) ;
#1093 = ORIENTED_EDGE ( 'NONE', *, *, #275, .T. ) ;
#1094 = EDGE_CURVE ( 'NONE', #4540, #13587, #9387, .T. ) ;
#1095 = EDGE_LOOP ( 'NONE', ( #4700, #8534, #7460, #13424, #596 ) ) ;
#1096 = CARTESIAN_POINT ( 'NONE',  ( -3.152801135295367096, -23.31250000136559564, -3.152801135295367541 ) ) ;
#1097 = DIRECTION ( 'NONE',  ( -0.000000000000000000, -1.000000000000000000, -0.000000000000000000 ) ) ;
#1098 = DIRECTION ( 'NONE',  ( 0.000000000000000000, 0.000000000000000000, -1.000000000000000000 ) ) ;
#1099 = CIRCLE ( 'NONE', #8348, 2.000000000000000888 ) ;
#1100 = DIRECTION ( 'NONE',  ( 0.000000000000000000, -1.000000000000000000, 0.000000000000000000 ) ) ;
#1101 = CARTESIAN_POINT ( 'NONE',  ( -5.725490332117415093, -5.000000000000000000, 22.00000000000001421 ) ) ;
#1102 = CARTESIAN_POINT ( 'NONE',  ( 3.061616997868383141E-16, -23.75000000000000000, -5.000000000000000000 ) ) ;
#1103 = CARTESIAN_POINT ( 'NONE',  ( -0.5711823568785978633, -5.381735091635035495, -2.312500000000001332 ) ) ;
#1104 = DIRECTION ( 'NONE',  ( 0.000000000000000000, 0.000000000000000000, 1.000000000000000000 ) ) ;
#1105 = LINE ( 'NONE', #10970, #4851 ) ;
#1106 = CARTESIAN_POINT ( 'NONE',  ( -4.458734124999999437, -26.93750000136559564, -5.460374474430324690E-16 ) ) ;
#1107 = CARTESIAN_POINT ( 'NONE',  ( -2.131511515620587272, -3.916244202832140253, -1.937499998634406584 ) ) ;
#1108 = VERTEX_POINT ( 'NONE', #2026 ) ;
#1109 = CIRCLE ( 'NONE', #8357, 4.250000000000000000 ) ;
#1110 = CARTESIAN_POINT ( 'NONE',  ( 3.061616997868383043E-15, -20.00000000000000000, 25.00000000000000000 ) ) ;
#1111 = ORIENTED_EDGE ( 'NONE', *, *, #5804, .F. ) ;
#1112 = ORIENTED_EDGE ( 'NONE', *, *, #2548, .T. ) ;
#1113 = CARTESIAN_POINT ( 'NONE',  ( -7.500000000000004441, -1.545780083834020102, -7.491787297939580981 ) ) ;
#1114 = EDGE_CURVE ( 'NONE', #794, #15817, #9839, .T. ) ;
#1115 = CARTESIAN_POINT ( 'NONE',  ( -4.458734125000001214, -24.87500000136559919, 1.846868145590734089 ) ) ;
#1116 = CARTESIAN_POINT ( 'NONE',  ( 5.000000000000004441, 6.350331166892669572E-15, -1.920263044861758583 ) ) ;
#1117 = ORIENTED_EDGE ( 'NONE', *, *, #12225, .T. ) ;
#1118 = DIRECTION ( 'NONE',  ( -0.000000000000000000, 1.000000000000000000, -0.000000000000000000 ) ) ;
#1119 = PRODUCT_DEFINITION_SHAPE ( 'NONE', 'NONE',  #15966 ) ;
#1120 = LINE ( 'NONE', #3465, #2794 ) ;
#1121 = DIRECTION ( 'NONE',  ( 0.000000000000000000, -0.000000000000000000, 1.000000000000000000 ) ) ;
#1122 = CARTESIAN_POINT ( 'NONE',  ( 0.000000000000000000, 0.000000000000000000, 0.000000000000000000 ) ) ;
#1123 = CARTESIAN_POINT ( 'NONE',  ( -3.152801135295367096, -25.31250000136559564, -3.152801135295367541 ) ) ;
#1124 = DIRECTION ( 'NONE',  ( 1.000000000000000000, 0.000000000000000000, -0.000000000000000000 ) ) ;
#1125 = APPLICATION_CONTEXT ( 'automotive_design' ) ;
#1126 = EDGE_CURVE ( 'NONE', #5812, #2885, #10679, .T. ) ;
#1127 = FACE_OUTER_BOUND ( 'NONE', #9552, .T. ) ;
#1128 = CARTESIAN_POINT ( 'NONE',  ( -5.000000000000095035, -0.7223674278660573433, -6.396799362785969834 ) ) ;
#1129 = DIRECTION ( 'NONE',  ( 0.000000000000000000, -0.000000000000000000, -1.000000000000000000 ) ) ;
#1130 = DIRECTION ( 'NONE',  ( 1.000000000000000000, 0.000000000000000000, 0.000000000000000000 ) ) ;
#1131 = ORIENTED_EDGE ( 'NONE', *, *, #15114, .T. ) ;
#1132 =( NAMED_UNIT ( * ) SI_UNIT ( $, .STERADIAN. ) SOLID_ANGLE_UNIT ( ) );
#1133 = ORIENTED_EDGE ( 'NONE', *, *, #3684, .T. ) ;
#1134 = CARTESIAN_POINT ( 'NONE',  ( 57.73502691896258199, -20.00000000000000000, 2.081668171172168513E-14 ) ) ;
#1135 = ORIENTED_EDGE ( 'NONE', *, *, #12438, .T. ) ;
#1136 = CARTESIAN_POINT ( 'NONE',  ( 0.000000000000000000, -13.00000000000000178, 0.000000000000000000 ) ) ;
#1137 =( GEOMETRIC_REPRESENTATION_CONTEXT ( 3 ) GLOBAL_UNCERTAINTY_ASSIGNED_CONTEXT ( ( #1398 ) ) GLOBAL_UNIT_ASSIGNED_CONTEXT ( ( #4736, #5875, #7019 ) ) REPRESENTATION_CONTEXT ( 'NONE', 'WORKASPACE' ) );
#1138 = AXIS2_PLACEMENT_3D ( 'NONE', #6971, #10753, #14236 ) ;
#1139 = FACE_OUTER_BOUND ( 'NONE', #10434, .T. ) ;
#1140 = EDGE_CURVE ( 'NONE', #4136, #11992, #9616, .T. ) ;
#1141 = CARTESIAN_POINT ( 'NONE',  ( 3.535533905932738197, -27.87500000000000000, -3.535533905932738197 ) ) ;
#1142 = ADVANCED_FACE ( 'NONE', ( #12113 ), #7524, .T. ) ;
#1143 = DIRECTION ( 'NONE',  ( 6.123233995736766036E-17, 1.000000000000000000, 0.000000000000000000 ) ) ;
#1144 = CARTESIAN_POINT ( 'NONE',  ( 3.916244202832140253, -2.131511515620588160, -1.687499998634406362 ) ) ;
#1145 = DIRECTION ( 'NONE',  ( 0.000000000000000000, 1.000000000000000000, 0.000000000000000000 ) ) ;
#1146 = CARTESIAN_POINT ( 'NONE',  ( 2.500000000000000000, 1.178949249685213863, -2.042000000000001148 ) ) ;
#1147 = CIRCLE ( 'NONE', #10202, 2.649999999999985700 ) ;
#1148 = ORIENTED_EDGE ( 'NONE', *, *, #5739, .F. ) ;
#1149 = CARTESIAN_POINT ( 'NONE',  ( 3.061616997868383141E-16, -26.75000000000000000, -5.000000000000000000 ) ) ;
#1150 = ORIENTED_EDGE ( 'NONE', *, *, #5943, .T. ) ;
#1151 = B_SPLINE_CURVE_WITH_KNOTS ( 'NONE', 3,
 ( #1741, #5774, #12799, #10712, #5703 ),
 .UNSPECIFIED., .F., .F.,
 ( 4, 1, 4 ),
 ( 0.000000000000000000, 0.002309401076758505790, 0.004618802153517011580 ),
 .UNSPECIFIED. ) ;
#1152 = ORIENTED_EDGE ( 'NONE', *, *, #13038, .F. ) ;
#1153 = CARTESIAN_POINT ( 'NONE',  ( 3.916244202832140253, -2.131511515620588160, -2.687499998634407028 ) ) ;
#1154 = FILL_AREA_STYLE ('',( #15648 ) ) ;
#1155 =( GEOMETRIC_REPRESENTATION_CONTEXT ( 3 ) GLOBAL_UNCERTAINTY_ASSIGNED_CONTEXT ( ( #5133 ) ) GLOBAL_UNIT_ASSIGNED_CONTEXT ( ( #12689, #7870, #525 ) ) REPRESENTATION_CONTEXT ( 'NONE', 'WORKASPACE' ) );
#1156 = ADVANCED_BREP_SHAPE_REPRESENTATION ( '', ( #14368, #3223 ), #1392 ) ;
#1157 = CIRCLE ( 'NONE', #15121, 2.000000000000000000 ) ;
#1158 = CARTESIAN_POINT ( 'NONE',  ( -19.99999999999956657, -11.00000000000000178, -2.499999999999120259 ) ) ;
#1159 = CARTESIAN_POINT ( 'NONE',  ( -113.6871902368262965, -110.1917077999038099, -17.50000000000000000 ) ) ;
#1160 = CARTESIAN_POINT ( 'NONE',  ( -7.500000000000000000, -4.330127018922196314, -9.999999999999998224 ) ) ;
#1161 = EDGE_CURVE ( 'NONE', #13011, #10876, #5502, .T. ) ;
#1162 = CARTESIAN_POINT ( 'NONE',  ( -5.000000000000000888, -29.68750000273118417, -2.071067811865475949 ) ) ;
#1163 = CARTESIAN_POINT ( 'NONE',  ( -5.381735091635034607, 0.5711823568785950878, -1.437499997268815832 ) ) ;
#1164 = CARTESIAN_POINT ( 'NONE',  ( -15.99999999999979217, -9.000000000000001776, -1.500000000000001110 ) ) ;
#1165 = CARTESIAN_POINT ( 'NONE',  ( -8.190561711645485556E-16, -25.93750000136559564, 4.458734124999999437 ) ) ;
#1166 = CARTESIAN_POINT ( 'NONE',  ( 4.458734124999997661, -22.50000000136559564, 1.846868145590737864 ) ) ;
#1167 = CARTESIAN_POINT ( 'NONE',  ( 3.753672977998667726, 3.033343224707664376, -6.249999998634408804 ) ) ;
#1168 = DIRECTION ( 'NONE',  ( -0.4999999999999993894, 2.324088772396453021E-16, -0.8660254037844390407 ) ) ;
#1169 = VERTEX_POINT ( 'NONE', #13399 ) ;
#1170 = EDGE_LOOP ( 'NONE', ( #3935, #2515, #6182 ) ) ;
#1171 = DIRECTION ( 'NONE',  ( 1.000000000000000000, 0.000000000000000000, 0.000000000000000000 ) ) ;
#1172 = ORIENTED_EDGE ( 'NONE', *, *, #6097, .F. ) ;
#1173 = CARTESIAN_POINT ( 'NONE',  ( -3.152801135295367985, -25.06250000136559564, 3.152801135295367096 ) ) ;
#1174 = CARTESIAN_POINT ( 'NONE',  ( -5.000000000000000000, -23.62500000273118772, -6.123233995736766282E-16 ) ) ;
#1175 = AXIS2_PLACEMENT_3D ( 'NONE', #12176, #78, #12343 ) ;
#1176 = EDGE_CURVE ( 'NONE', #13609, #12316, #3175, .T. ) ;
#1177 = CARTESIAN_POINT ( 'NONE',  ( 35.00000000000000000, 37.00000000000000000, 5.999999999999991118 ) ) ;
#1178 = CARTESIAN_POINT ( 'NONE',  ( 3.750000000000004441, -6.495190528383289141, 0.000000000000000000 ) ) ;
#1179 = EDGE_CURVE ( 'NONE', #12690, #11826, #3166, .T. ) ;
#1180 = EDGE_CURVE ( 'NONE', #9048, #13189, #4457, .T. ) ;
#1181 = EDGE_CURVE ( 'NONE', #6165, #13829, #13462, .T. ) ;
#1182 = CARTESIAN_POINT ( 'NONE',  ( 2.500000000000000000, 2.357898499370433054, -1.951563910473907981E-15 ) ) ;
#1183 = AXIS2_PLACEMENT_3D ( 'NONE', #8469, #10583, #14590 ) ;
#1184 = CARTESIAN_POINT ( 'NONE',  ( -2.390265326283148806, -4.391654775818394363, -2.375000000000002220 ) ) ;
#1185 = CARTESIAN_POINT ( 'NONE',  ( -4.795541693661363958, -1.415196051561583790, -2.374999997268815388 ) ) ;
#1186 = CARTESIAN_POINT ( 'NONE',  ( 3.585155863502412998, -3.448070198354993732, -0.02305246973459410681 ) ) ;
#1187 = CARTESIAN_POINT ( 'NONE',  ( 4.458734125000000326, -26.37500000136559564, -1.846868145590734978 ) ) ;
#1188 = CIRCLE ( 'NONE', #14094, 2.649999999999985700 ) ;
#1189 = CARTESIAN_POINT ( 'NONE',  ( 2.131511515620586383, 3.916244202832140253, -3.437499998634407916 ) ) ;
#1190 = EDGE_LOOP ( 'NONE', ( #4329, #9452, #7570 ) ) ;
#1191 = VECTOR ( 'NONE', #6258, 1000.000000000000114 ) ;
#1192 = DIRECTION ( 'NONE',  ( -0.000000000000000000, -0.000000000000000000, -1.000000000000000000 ) ) ;
#1193 = ORIENTED_EDGE ( 'NONE', *, *, #1975, .T. ) ;
#1194 = EDGE_LOOP ( 'NONE', ( #577, #15095 ) ) ;
#1195 = DIRECTION ( 'NONE',  ( -1.000000000000000000, 0.000000000000000000, -0.000000000000000000 ) ) ;
#1196 = CARTESIAN_POINT ( 'NONE',  ( -1.846868145590737420, -23.75000000136559208, 4.458734124999999437 ) ) ;
#1197 = DIRECTION ( 'NONE',  ( -1.000000000000000000, -0.000000000000000000, -0.000000000000000000 ) ) ;
#1198 = VECTOR ( 'NONE', #14102, 1000.000000000000000 ) ;
#1199 = ORIENTED_EDGE ( 'NONE', *, *, #13990, .T. ) ;
#1200 = CARTESIAN_POINT ( 'NONE',  ( -81.33974596215560382, -110.0591436588189538, -7.500000000000000000 ) ) ;
#1201 = CARTESIAN_POINT ( 'NONE',  ( 3.033343224707661712, -3.753672977998669946, -3.749999998634409692 ) ) ;
#1202 = AXIS2_PLACEMENT_3D ( 'NONE', #273, #7860, #13980 ) ;
#1203 = DIRECTION ( 'NONE',  ( 1.000000000000000000, 0.000000000000000000, -0.000000000000000000 ) ) ;
#1204 = CARTESIAN_POINT ( 'NONE',  ( 6.000000000000000000, -20.00000000000000000, 1.500000000000000000 ) ) ;
#1205 = FACE_OUTER_BOUND ( 'NONE', #4446, .T. ) ;
#1206 = EDGE_CURVE ( 'NONE', #8828, #2328, #11225, .T. ) ;
#1207 = CARTESIAN_POINT ( 'NONE',  ( 2.730187237215162345E-16, -25.43750000136559564, -4.458734124999999437 ) ) ;
#1208 = FACE_OUTER_BOUND ( 'NONE', #14300, .T. ) ;
#1209 = AXIS2_PLACEMENT_3D ( 'NONE', #7335, #14454, #13290 ) ;
#1210 = CARTESIAN_POINT ( 'NONE',  ( -2.390265326283148806, -4.391654775818394363, -1.249999997268814278 ) ) ;
#1211 = CARTESIAN_POINT ( 'NONE',  ( -5.000000000000000888, -28.68750000273119127, -2.071067811865475949 ) ) ;
#1212 = CARTESIAN_POINT ( 'NONE',  ( 4.000000000000000000, 2.309401076758497151, -3.433295621305379353 ) ) ;
#1213 = DIRECTION ( 'NONE',  ( 0.000000000000000000, 0.4999999999999993894, -0.8660254037844389297 ) ) ;
#1214 = VERTEX_POINT ( 'NONE', #3633 ) ;
#1215 = ORIENTED_EDGE ( 'NONE', *, *, #14990, .T. ) ;
#1216 = DIRECTION ( 'NONE',  ( 0.000000000000000000, -0.5000000000000012212, -0.8660254037844380415 ) ) ;
#1217 = ORIENTED_EDGE ( 'NONE', *, *, #14351, .T. ) ;
#1218 = CARTESIAN_POINT ( 'NONE',  ( 5.000000000000000888, 0.000000000000000000, 0.000000000000000000 ) ) ;
#1219 = CIRCLE ( 'NONE', #5862, 5.000000000000000000 ) ;
#1220 = DIRECTION ( 'NONE',  ( -1.000000000000000000, -0.000000000000000000, -0.000000000000000000 ) ) ;
#1221 = VECTOR ( 'NONE', #2375, 1000.000000000000000 ) ;
#1222 = CARTESIAN_POINT ( 'NONE',  ( 4.799145180956616130, -0.5093500532425063732, -2.374999998634407028 ) ) ;
#1223 = APPLICATION_PROTOCOL_DEFINITION ( 'draft international standard', 'automotive_design', 1998, #4001 ) ;
#1224 = CARTESIAN_POINT ( 'NONE',  ( 3.916244202832140253, -2.131511515620588160, -4.687499998634405252 ) ) ;
#1225 = AXIS2_PLACEMENT_3D ( 'NONE', #6934, #1826, #1750 ) ;
#1226 = FACE_OUTER_BOUND ( 'NONE', #7970, .T. ) ;
#1227 = CARTESIAN_POINT ( 'NONE',  ( -41.99999999999978684, -11.00000000000000178, 3.499999999999998668 ) ) ;
#1228 = ORIENTED_EDGE ( 'NONE', *, *, #10879, .T. ) ;
#1229 = CARTESIAN_POINT ( 'NONE',  ( 9.999999999999891642, -20.00000000000000000, -17.32050807568883499 ) ) ;
#1230 = ORIENTED_EDGE ( 'NONE', *, *, #3922, .T. ) ;
#1231 = VECTOR ( 'NONE', #11987, 1000.000000000000000 ) ;
#1232 = VERTEX_POINT ( 'NONE', #12353 ) ;
#1233 = CONTEXT_DEPENDENT_SHAPE_REPRESENTATION ( #5263, #12939 ) ;
#1234 = CARTESIAN_POINT ( 'NONE',  ( -3.753672977998669502, -3.033343224707661712, -3.999999998634410137 ) ) ;
#1235 = ADVANCED_FACE ( 'NONE', ( #10 ), #1285, .F. ) ;
#1236 = EDGE_CURVE ( 'NONE', #10448, #4594, #4927, .T. ) ;
#1237 = FACE_OUTER_BOUND ( 'NONE', #12435, .T. ) ;
#1238 = VECTOR ( 'NONE', #13025, 1000.000000000000000 ) ;
#1239 = DIRECTION ( 'NONE',  ( 1.000000000000000000, 0.000000000000000000, 0.000000000000000000 ) ) ;
#1240 = CARTESIAN_POINT ( 'NONE',  ( 2.143131898507869826E-15, 50.00000000000000000, -67.50000000000000000 ) ) ;
#1241 = CARTESIAN_POINT ( 'NONE',  ( 4.391654775818395251, -2.390265326283149694, -2.125000000000001776 ) ) ;
#1242 = VECTOR ( 'NONE', #8938, 1000.000000000000000 ) ;
#1243 = CARTESIAN_POINT ( 'NONE',  ( 5.000000000000000000, -27.18750000273119127, 2.071067811865478614 ) ) ;
#1244 = VECTOR ( 'NONE', #15908, 1000.000000000000000 ) ;
#1245 = CARTESIAN_POINT ( 'NONE',  ( 3.401574460001763001, -4.209348295687703967, -0.06249999726881655393 ) ) ;
#1246 = CARTESIAN_POINT ( 'NONE',  ( -2.000000000000007550, -3.464101615137749945, 0.000000000000000000 ) ) ;
#1247 = CARTESIAN_POINT ( 'NONE',  ( -0.7119955712286091254, 4.450395979295969973, -0.3533432011777784543 ) ) ;
#1248 = CARTESIAN_POINT ( 'NONE',  ( -1.846868145590734756, -27.37500000136559564, -4.458734124999999437 ) ) ;
#1249 = CARTESIAN_POINT ( 'NONE',  ( -3.152801135295367985, -22.81250000136559564, 3.152801135295367096 ) ) ;
#1250 = CARTESIAN_POINT ( 'NONE',  ( -3.753672977998669946, -3.033343224707661712, -2.749999998634409248 ) ) ;
#1251 = LINE ( 'NONE', #6199, #8673 ) ;
#1252 = ORIENTED_EDGE ( 'NONE', *, *, #10295, .F. ) ;
#1253 = AXIS2_PLACEMENT_3D ( 'NONE', #297, #13847, #4963 ) ;
#1254 = ORIENTED_EDGE ( 'NONE', *, *, #1180, .T. ) ;
#1255 = VECTOR ( 'NONE', #10833, 1000.000000000000000 ) ;
#1256 =( LENGTH_UNIT ( ) NAMED_UNIT ( * ) SI_UNIT ( .MILLI., .METRE. ) );
#1257 = ORIENTED_EDGE ( 'NONE', *, *, #4707, .F. ) ;
#1258 = CARTESIAN_POINT ( 'NONE',  ( -8.190561711645485556E-16, -21.93750000136559208, 4.458734124999999437 ) ) ;
#1259 = EDGE_CURVE ( 'NONE', #10280, #10210, #6230, .T. ) ;
#1260 = DIRECTION ( 'NONE',  ( 0.000000000000000000, 1.000000000000000000, 0.000000000000000000 ) ) ;
#1261 = EDGE_CURVE ( 'NONE', #11117, #5376, #7210, .T. ) ;
#1262 = B_SPLINE_CURVE_WITH_KNOTS ( 'NONE', 3,
 ( #15673, #10735, #9525, #12006, #6785, #4434 ),
 .UNSPECIFIED., .F., .F.,
 ( 4, 2, 4 ),
 ( -3.640115492407174633E-06, 0.0002066546034006553863, 0.0004169493222937179812 ),
 .UNSPECIFIED. ) ;
#1263 = FACE_BOUND ( 'NONE', #7017, .T. ) ;
#1264 = LINE ( 'NONE', #1177, #4309 ) ;
#1265 = CARTESIAN_POINT ( 'NONE',  ( 2.500000000000000000, -1.178949249685218303, -2.041999999999998039 ) ) ;
#1266 = CIRCLE ( 'NONE', #10326, 5.000000000000000000 ) ;
#1267 = CARTESIAN_POINT ( 'NONE',  ( -4.391654775818395251, 2.390265326283148806, -1.625000000000001332 ) ) ;
#1268 = CARTESIAN_POINT ( 'NONE',  ( 4.391654775818395251, -2.390265326283149694, -1.999999997268814944 ) ) ;
#1269 = CARTESIAN_POINT ( 'NONE',  ( -3.864322703872500764, -2.771540215593305323, -0.1764184119287106334 ) ) ;
#1270 = CARTESIAN_POINT ( 'NONE',  ( 3.152801135295367541, -26.31250000136559564, -3.152801135295367541 ) ) ;
#1271 = CARTESIAN_POINT ( 'NONE',  ( -1.261996585732579224, 4.276409079477648589, -4.312499998634405252 ) ) ;
#1272 = ORIENTED_EDGE ( 'NONE', *, *, #15927, .T. ) ;
#1273 = CARTESIAN_POINT ( 'NONE',  ( -7.500000000000000888, -4.330127018922199866, -1.000000000000000888 ) ) ;
#1274 = ORIENTED_EDGE ( 'NONE', *, *, #11198, .T. ) ;
#1275 = VERTEX_POINT ( 'NONE', #12264 ) ;
#1276 = CARTESIAN_POINT ( 'NONE',  ( -55.00000000000000000, -1.734723475976807094E-15, 17.50000000000000000 ) ) ;
#1277 = CARTESIAN_POINT ( 'NONE',  ( 1.846868145590735200, -25.25000000136559564, -4.458734125000000326 ) ) ;
#1278 = EDGE_CURVE ( 'NONE', #482, #13637, #7445, .T. ) ;
#1279 = DIRECTION ( 'NONE',  ( 1.000000000000000000, 0.000000000000000000, 0.000000000000000000 ) ) ;
#1280 = EDGE_CURVE ( 'NONE', #14345, #6321, #604, .T. ) ;
#1281 = ORIENTED_EDGE ( 'NONE', *, *, #8662, .T. ) ;
#1282 = CARTESIAN_POINT ( 'NONE',  ( 42.02221399786069611, -3.000000000000000000, 1.040834085586084257E-13 ) ) ;
#1283 = CARTESIAN_POINT ( 'NONE',  ( 4.613983237546154470, -6.452243898629821395, -7.591546097228405898 ) ) ;
#1284 = CARTESIAN_POINT ( 'NONE',  ( -0.6448876103708541807, -4.246476118072358474, -0.2256878752776773356 ) ) ;
#1285 = CYLINDRICAL_SURFACE ( 'NONE', #6526, 2.649999999999992806 ) ;
#1286 = CARTESIAN_POINT ( 'NONE',  ( 1.846868145590735200, -24.50000000136559564, -4.458734125000000326 ) ) ;
#1287 = DIRECTION ( 'NONE',  ( 0.000000000000000000, 0.000000000000000000, 1.000000000000000000 ) ) ;
#1288 = FACE_BOUND ( 'NONE', #3074, .T. ) ;
#1289 = CARTESIAN_POINT ( 'NONE',  ( 3.535533905932738197, -28.00000000273118772, -3.535533905932738197 ) ) ;
#1290 = DIRECTION ( 'NONE',  ( 0.000000000000000000, 0.000000000000000000, -1.000000000000000000 ) ) ;
#1291 = CARTESIAN_POINT ( 'NONE',  ( -4.458734124999999437, -29.00000000136559564, -1.846868145590735644 ) ) ;
#1292 = SURFACE_STYLE_USAGE ( .BOTH. , #9862 ) ;
#1293 = ORIENTED_EDGE ( 'NONE', *, *, #14089, .T. ) ;
#1294 =( BOUNDED_CURVE ( )  B_SPLINE_CURVE ( 2, ( #15589, #13146, #12302, #14666, #6099, #4506, #9443, #12144, #3592 ),
 .UNSPECIFIED., .F., .F. ) 
 B_SPLINE_CURVE_WITH_KNOTS ( ( 3, 2, 2, 2, 3 ),
 ( 0.2250000000000001998, 0.2375000000000000999, 0.2500000000000000555, 0.2624999999999999556, 0.2749999999999999112 ),
 .UNSPECIFIED. ) 
 CURVE ( )  GEOMETRIC_REPRESENTATION_ITEM ( )  RATIONAL_B_SPLINE_CURVE ( ( 0.9999999999999987788, 0.9238795325112879597, 1.000000000000000000, 0.9238795325112867385, 1.000000000000000000, 0.9238795325112867385, 1.000000000000000000, 0.9238795325112874046, 0.9999999999999993339 ) ) 
 REPRESENTATION_ITEM ( '' )  );
#1296 = EDGE_CURVE ( 'NONE', #10322, #15077, #2338, .T. ) ;
#1295 = ORIENTED_EDGE ( 'NONE', *, *, #8606, .T. ) ;
#1297 = CARTESIAN_POINT ( 'NONE',  ( -5.725490332106780933, -3.000000000000000000, -9.916840153467775920 ) ) ;
#1298 = ADVANCED_FACE ( 'NONE', ( #12183 ), #6541, .T. ) ;
#1299 = ORIENTED_EDGE ( 'NONE', *, *, #3275, .F. ) ;
#1300 = DIRECTION ( 'NONE',  ( 0.000000000000000000, 0.000000000000000000, -1.000000000000000000 ) ) ;
#1301 = CARTESIAN_POINT ( 'NONE',  ( 40.53089410526170866, -3.098194602941708009, 27.46587016624057753 ) ) ;
#1302 = CARTESIAN_POINT ( 'NONE',  ( 0.5093500532425063732, 4.799145180956616130, -4.124999998634405252 ) ) ;
#1303 = APPLICATION_PROTOCOL_DEFINITION ( 'draft international standard', 'automotive_design', 1998, #14873 ) ;
#1304 = CARTESIAN_POINT ( 'NONE',  ( 3.033343224707661712, -3.753672977998669946, -5.749999998634407916 ) ) ;
#1305 = DIRECTION ( 'NONE',  ( 0.000000000000000000, 0.000000000000000000, 1.000000000000000000 ) ) ;
#1306 = DIRECTION ( 'NONE',  ( -0.8660254037844407060, 0.4999999999999965583, 0.000000000000000000 ) ) ;
#1307 = VERTEX_POINT ( 'NONE', #10989 ) ;
#1308 = DIRECTION ( 'NONE',  ( 0.000000000000000000, 1.000000000000000000, 0.000000000000000000 ) ) ;
#1309 = SHAPE_REPRESENTATION_RELATIONSHIP ( 'NONE' , 'NONE' ,  #3049, #6582 ) ;
#1310 = ORIENTED_EDGE ( 'NONE', *, *, #5864, .F. ) ;
#1311 = DIRECTION ( 'NONE',  ( 0.000000000000000000, -0.5000000000000011102, -0.8660254037844379305 ) ) ;
#1312 = CARTESIAN_POINT ( 'NONE',  ( 31.75426480542942898, -37.00000000000000711, -14.99999999999999645 ) ) ;
#1313 = ADVANCED_FACE ( 'NONE', ( #4853, #14711, #7357, #1205, #6151 ), #85, .F. ) ;
#1314 = ORIENTED_EDGE ( 'NONE', *, *, #10414, .F. ) ;
#1315 = ITEM_DEFINED_TRANSFORMATION ( 'NONE', 'NONE', #9661,  #3223 ) ;
#1316 = CARTESIAN_POINT ( 'NONE',  ( 3.916244202832140253, -2.131511515620588160, -1.687499998634406362 ) ) ;
#1317 = CYLINDRICAL_SURFACE ( 'NONE', #10718, 2.649999999999992806 ) ;
#1318 = PRODUCT_DEFINITION_SHAPE ( 'NONE', 'NONE',  #15983 ) ;
#1319 = DIRECTION ( 'NONE',  ( 0.000000000000000000, 0.000000000000000000, 1.000000000000000000 ) ) ;
#1320 = CARTESIAN_POINT ( 'NONE',  ( 4.729367062499999719, -31.28125000204839168, 0.000000000000000000 ) ) ;
#1321 = LINE ( 'NONE', #13758, #7982 ) ;
#1322 = CARTESIAN_POINT ( 'NONE',  ( -4.795541693661363958, -1.415196051561583790, -2.374999997268815388 ) ) ;
#1323 = FACE_OUTER_BOUND ( 'NONE', #7151, .T. ) ;
#1324 = ADVANCED_FACE ( 'NONE', ( #11618 ), #4190, .F. ) ;
#1325 = CARTESIAN_POINT ( 'NONE',  ( 5.000000000000003553, 1.275685995473128912E-14, -4.920263044861760804 ) ) ;
#1326 = CARTESIAN_POINT ( 'NONE',  ( -1.846868145590737420, -24.00000000136559564, 4.458734124999997661 ) ) ;
#1327 = ORIENTED_EDGE ( 'NONE', *, *, #11619, .T. ) ;
#1328 = CARTESIAN_POINT ( 'NONE',  ( 4.458734124999999437, -23.37500000136559564, -1.846868145590734978 ) ) ;
#1329 = CARTESIAN_POINT ( 'NONE',  ( -3.753672977998669946, -3.033343224707661712, -3.749999998634409692 ) ) ;
#1330 = CARTESIAN_POINT ( 'NONE',  ( 6.123233995736766282E-16, -20.00000000000000000, -5.000000000000000000 ) ) ;
#1331 = ORIENTED_EDGE ( 'NONE', *, *, #15514, .F. ) ;
#1332 = ORIENTED_EDGE ( 'NONE', *, *, #2188, .T. ) ;
#1333 = AXIS2_PLACEMENT_3D ( 'NONE', #14314, #3242, #9613 ) ;
#1334 = ORIENTED_EDGE ( 'NONE', *, *, #11046, .T. ) ;
#1335 = CARTESIAN_POINT ( 'NONE',  ( 2.071067811865473285, -30.93750000273118417, -5.000000000000002665 ) ) ;
#1336 = DIRECTION ( 'NONE',  ( -0.000000000000000000, 1.000000000000000000, -0.000000000000000000 ) ) ;
#1337 = CARTESIAN_POINT ( 'NONE',  ( -9.184850993605147944E-16, -22.25000000000000000, 5.000000000000000000 ) ) ;
#1338 = DIRECTION ( 'NONE',  ( -0.000000000000000000, 1.000000000000000000, -0.000000000000000000 ) ) ;
#1339 = CARTESIAN_POINT ( 'NONE',  ( -1.250000000000010436, 7.938566201357381225, -7.198902722707439139 ) ) ;
#1340 = CARTESIAN_POINT ( 'NONE',  ( -5.000000000000004441, -7.530481206757679743E-15, -1.545263047592943861 ) ) ;
#1341 = CARTESIAN_POINT ( 'NONE',  ( 4.391654775818395251, -2.390265326283149694, -4.125000000000000000 ) ) ;
#1342 = CARTESIAN_POINT ( 'NONE',  ( 5.000000000000093259, 0.7223674278660628945, -4.021799365517152225 ) ) ;
#1343 = EDGE_CURVE ( 'NONE', #4219, #74, #1876, .T. ) ;
#1344 = DIRECTION ( 'NONE',  ( 1.319090325525611458E-16, 1.000000000000000000, -0.000000000000000000 ) ) ;
#1345 = ADVANCED_FACE ( 'NONE', ( #14048 ), #6389, .F. ) ;
#1346 = CARTESIAN_POINT ( 'NONE',  ( 4.458734124999999437, -26.43750000136559564, 0.000000000000000000 ) ) ;
#1347 = CARTESIAN_POINT ( 'NONE',  ( 4.276409079477644148, 1.261996585732577891, -2.562499998634407028 ) ) ;
#1348 = ORIENTED_EDGE ( 'NONE', *, *, #4910, .F. ) ;
#1349 = LINE ( 'NONE', #2473, #9954 ) ;
#1350 = ORIENTED_EDGE ( 'NONE', *, *, #12395, .F. ) ;
#1351 = ORIENTED_EDGE ( 'NONE', *, *, #2624, .F. ) ;
#1352 = DIRECTION ( 'NONE',  ( 0.000000000000000000, 1.000000000000000000, 0.000000000000000000 ) ) ;
#1353 = CARTESIAN_POINT ( 'NONE',  ( -3.152801135295367096, -26.06250000136559564, -3.152801135295367541 ) ) ;
#1354 = DIRECTION ( 'NONE',  ( 0.000000000000000000, 1.000000000000000000, 0.000000000000000000 ) ) ;
#1355 = ORIENTED_EDGE ( 'NONE', *, *, #10703, .F. ) ;
#1356 = DIRECTION ( 'NONE',  ( -0.000000000000000000, -1.000000000000000000, -0.000000000000000000 ) ) ;
#1357 = CIRCLE ( 'NONE', #9608, 10.39117206796836079 ) ;
#1358 = CARTESIAN_POINT ( 'NONE',  ( -60.00000000000000000, 88.59290746114278647, -18.00000000000001066 ) ) ;
#1359 = CARTESIAN_POINT ( 'NONE',  ( 0.5093500532425063732, 4.799145180956616130, -3.124999998634407472 ) ) ;
#1360 = DIRECTION ( 'NONE',  ( -0.000000000000000000, 0.000000000000000000, 1.000000000000000000 ) ) ;
#1361 = CARTESIAN_POINT ( 'NONE',  ( -2.071067811865478170, -28.31250000000000355, 5.000000000000000000 ) ) ;
#1362 = FACE_OUTER_BOUND ( 'NONE', #8809, .T. ) ;
#1363 = EDGE_CURVE ( 'NONE', #10448, #13539, #8407, .T. ) ;
#1364 = CARTESIAN_POINT ( 'NONE',  ( 2.500000000000000000, 0.000000000000000000, 0.000000000000000000 ) ) ;
#1365 = ADVANCED_FACE ( 'NONE', ( #259 ), #12501, .T. ) ;
#1366 = CARTESIAN_POINT ( 'NONE',  ( -5.000000000000000888, -28.56250000273118417, 2.071067811865474617 ) ) ;
#1367 = CARTESIAN_POINT ( 'NONE',  ( 1.306442393143573577, 8.377108146505383601, -7.792327460285856766 ) ) ;
#1368 = CARTESIAN_POINT ( 'NONE',  ( 3.152801135295367541, -30.31250000136559564, -3.152801135295367541 ) ) ;
#1369 = LINE ( 'NONE', #10033, #13813 ) ;
#1370 = ORIENTED_EDGE ( 'NONE', *, *, #10083, .T. ) ;
#1371 = EDGE_LOOP ( 'NONE', ( #10340, #15637, #15181, #9864 ) ) ;
#1372 = ORIENTED_EDGE ( 'NONE', *, *, #14448, .F. ) ;
#1373 = CARTESIAN_POINT ( 'NONE',  ( 7.500000000000001776, 4.330127018922190985, -7.564338275809340928 ) ) ;
#1374 = ORIENTED_EDGE ( 'NONE', *, *, #4282, .F. ) ;
#1375 = CARTESIAN_POINT ( 'NONE',  ( 4.197393957002303999, 7.772902908466098641E-14, -3.503767560748929810 ) ) ;
#1376 = CIRCLE ( 'NONE', #12467, 5.000000000000001776 ) ;
#1377 = CARTESIAN_POINT ( 'NONE',  ( 1.846868145590735200, -31.50000000136559564, -4.458734125000000326 ) ) ;
#1378 = EDGE_CURVE ( 'NONE', #15644, #3643, #6798, .T. ) ;
#1379 = CARTESIAN_POINT ( 'NONE',  ( -0.5093500532425060401, -4.799145180956616130, -4.624999998634405252 ) ) ;
#1380 = ADVANCED_FACE ( 'NONE', ( #7774 ), #6544, .F. ) ;
#1381 = DIRECTION ( 'NONE',  ( 6.123233995736766036E-17, -1.000000000000000000, 0.000000000000000000 ) ) ;
#1382 =( BOUNDED_CURVE ( )  B_SPLINE_CURVE ( 2, ( #3828, #7804, #6427, #8687, #12696, #2771, #8848, #12624, #13924, #7643, #2687 ),
 .UNSPECIFIED., .F., .F. ) 
 B_SPLINE_CURVE_WITH_KNOTS ( ( 3, 2, 2, 2, 2, 3 ),
 ( 0.5545872658012773737, 0.5625000000000000000, 0.5749999999999999556, 0.5875000000000000222, 0.5999999999999999778, 0.6045872658012773071 ),
 .UNSPECIFIED. ) 
 CURVE ( )  GEOMETRIC_REPRESENTATION_ITEM ( )  RATIONAL_B_SPLINE_CURVE ( ( 0.9646335149384803742, 0.9518143178943441196, 1.000000000000000000, 0.9238795325112867385, 1.000000000000000000, 0.9238795325112867385, 1.000000000000000000, 0.9238795325112867385, 1.000000000000000000, 0.9720652146169428409, 0.9646335149384808183 ) ) 
 REPRESENTATION_ITEM ( '' )  );
#1383 = EDGE_CURVE ( 'NONE', #138, #615, #4026, .T. ) ;
#1384 = CARTESIAN_POINT ( 'NONE',  ( -0.5093500532425060401, -4.799145180956616130, -4.874999998634405252 ) ) ;
#1385 = CARTESIAN_POINT ( 'NONE',  ( -39.99999999999999289, -9.000000000000001776, 8.300651832549021947E-13 ) ) ;
#1386 = PLANE ( 'NONE',  #9760 ) ;
#1387 = ORIENTED_EDGE ( 'NONE', *, *, #5738, .T. ) ;
#1388 = CARTESIAN_POINT ( 'NONE',  ( -7.500000000000003553, -1.084202172485504434E-15, -6.991905250253755533 ) ) ;
#1389 = VERTEX_POINT ( 'NONE', #15196 ) ;
#1390 = CARTESIAN_POINT ( 'NONE',  ( 45.58845726811992449, 88.59290746114278647, -42.96152422706630603 ) ) ;
#1391 = LINE ( 'NONE', #1312, #701 ) ;
#1392 =( GEOMETRIC_REPRESENTATION_CONTEXT ( 3 ) GLOBAL_UNCERTAINTY_ASSIGNED_CONTEXT ( ( #13859 ) ) GLOBAL_UNIT_ASSIGNED_CONTEXT ( ( #13328, #11002, #7290 ) ) REPRESENTATION_CONTEXT ( 'NONE', 'WORKASPACE' ) );
#1393 = ORIENTED_EDGE ( 'NONE', *, *, #6464, .T. ) ;
#1394 = CARTESIAN_POINT ( 'NONE',  ( -4.276409079477644148, -1.261996585732578335, -7.062499998634407916 ) ) ;
#1395 = AXIS2_PLACEMENT_3D ( 'NONE', #13554, #2487, #7448 ) ;
#1396 = CARTESIAN_POINT ( 'NONE',  ( -2.687328764639638656, 3.067272167851286202, -0.05923475698270370959 ) ) ;
#1397 = CARTESIAN_POINT ( 'NONE',  ( 0.000000000000000000, -32.00000000000000000, 0.000000000000000000 ) ) ;
#1398 = UNCERTAINTY_MEASURE_WITH_UNIT (LENGTH_MEASURE( 1.000000000000000082E-05 ), #4736, 'distance_accuracy_value', 'NONE');
#1399 = EDGE_CURVE ( 'NONE', #3787, #13461, #8894, .T. ) ;
#1400 = CARTESIAN_POINT ( 'NONE',  ( -9.184850993605147944E-16, -30.37500000273118772, 5.000000000000000000 ) ) ;
#1401 = AXIS2_PLACEMENT_3D ( 'NONE', #6117, #4901, #11119 ) ;
#1402 = CARTESIAN_POINT ( 'NONE',  ( -0.5711823568785978633, -5.381735091635035495, -5.187499997268819385 ) ) ;
#1403 = CARTESIAN_POINT ( 'NONE',  ( 2.390265326283148806, 4.391654775818395251, -8.749999997268814056 ) ) ;
#1404 = CARTESIAN_POINT ( 'NONE',  ( 0.2565871882082941813, 4.472639628789296218, -0.3724480747979372897 ) ) ;
#1405 = CARTESIAN_POINT ( 'NONE',  ( 4.458734124999999437, -25.68750000136559564, 0.000000000000000000 ) ) ;
#1406 = EDGE_LOOP ( 'NONE', ( #6205, #15290, #10257, #9032, #4103 ) ) ;
#1407 = PRESENTATION_LAYER_ASSIGNMENT (  '', '', ( #7352 ) ) ;
#1408 = CARTESIAN_POINT ( 'NONE',  ( -28.86751345948129810, -3.000000000000000000, 22.00000000000000711 ) ) ;
#1409 = CARTESIAN_POINT ( 'NONE',  ( -0.5093500532425060401, -4.799145180956616130, -7.624999998634408804 ) ) ;
#1410 = CARTESIAN_POINT ( 'NONE',  ( 25.00000000000000000, 0.000000000000000000, 0.000000000000000000 ) ) ;
#1411 = VERTEX_POINT ( 'NONE', #12825 ) ;
#1412 = EDGE_LOOP ( 'NONE', ( #9601, #5953, #4082, #1598 ) ) ;
#1413 = CARTESIAN_POINT ( 'NONE',  ( 0.000000000000000000, 0.000000000000000000, 0.000000000000000000 ) ) ;
#1414 = ORIENTED_EDGE ( 'NONE', *, *, #10465, .T. ) ;
#1415 = CARTESIAN_POINT ( 'NONE',  ( -5.276765049035074817, 6.073111908730299824, -7.634085501268424778 ) ) ;
#1416 = FACE_BOUND ( 'NONE', #3456, .T. ) ;
#1417 = AXIS2_PLACEMENT_3D ( 'NONE', #14635, #4617, #15541 ) ;
#1418 = DIRECTION ( 'NONE',  ( -0.000000000000000000, -0.000000000000000000, 1.000000000000000000 ) ) ;
#1419 = ADVANCED_FACE ( 'NONE', ( #7691 ), #1687, .F. ) ;
#1420 = STYLED_ITEM ( 'NONE', ( #5368 ), #14097 ) ;
#1421 = CARTESIAN_POINT ( 'NONE',  ( -7.500000000000000000, -4.330127018922196314, -7.422398894150035176 ) ) ;
#1422 = CARTESIAN_POINT ( 'NONE',  ( -5.147825380260984574, -5.688155668809796062, -7.450218641349908744 ) ) ;
#1423 = DIRECTION ( 'NONE',  ( -1.000000000000000000, 0.000000000000000000, 0.000000000000000000 ) ) ;
#1424 = CARTESIAN_POINT ( 'NONE',  ( 4.209348295687701302, 3.401574460001765665, -3.937500000000000888 ) ) ;
#1425 = CARTESIAN_POINT ( 'NONE',  ( -5.000000000000004441, -7.530481206757679743E-15, -2.545263047592944972 ) ) ;
#1426 = CARTESIAN_POINT ( 'NONE',  ( 0.02511973781850649831, -4.877415612947427981, -3.751298745799844792 ) ) ;
#1427 = CARTESIAN_POINT ( 'NONE',  ( -4.458734125000000326, -27.00000000136559208, -1.846868145590735644 ) ) ;
#1428 = CARTESIAN_POINT ( 'NONE',  ( -3.916244202832140253, 2.131511515620587272, -2.187499998634407028 ) ) ;
#1429 = ORIENTED_EDGE ( 'NONE', *, *, #14917, .F. ) ;
#1430 = PRESENTATION_LAYER_ASSIGNMENT (  '', '', ( #14079 ) ) ;
#1431 = CARTESIAN_POINT ( 'NONE',  ( -7.897836333153811950, -1.530409084195006653, -7.633857274177628938 ) ) ;
#1432 = ORIENTED_EDGE ( 'NONE', *, *, #15632, .T. ) ;
#1433 = ORIENTED_EDGE ( 'NONE', *, *, #292, .F. ) ;
#1434 = AXIS2_PLACEMENT_3D ( 'NONE', #9682, #10829, #12021 ) ;
#1435 = CARTESIAN_POINT ( 'NONE',  ( 2.730187237215162345E-16, -24.18750000136559564, -4.458734124999999437 ) ) ;
#1436 = DIRECTION ( 'NONE',  ( 0.8660254037844383745, 0.000000000000000000, 0.5000000000000004441 ) ) ;
#1437 = ORIENTED_EDGE ( 'NONE', *, *, #6878, .T. ) ;
#1438 = CARTESIAN_POINT ( 'NONE',  ( -4.000000000000000000, -1.560351142792950618, -0.2242961665059814425 ) ) ;
#1439 = EDGE_CURVE ( 'NONE', #2989, #10378, #3177, .T. ) ;
#1440 = EDGE_CURVE ( 'NONE', #580, #15000, #2895, .T. ) ;
#1441 = VECTOR ( 'NONE', #12812, 1000.000000000000000 ) ;
#1442 = DIRECTION ( 'NONE',  ( 0.000000000000000000, 0.000000000000000000, 1.000000000000000000 ) ) ;
#1443 = PLANE ( 'NONE',  #5897 ) ;
#1444 = DIRECTION ( 'NONE',  ( -0.000000000000000000, 1.000000000000000000, -0.000000000000000000 ) ) ;
#1445 = VECTOR ( 'NONE', #11850, 1000.000000000000000 ) ;
#1446 = CARTESIAN_POINT ( 'NONE',  ( -3.535533905932738641, -31.37500000000000000, 3.535533905932737309 ) ) ;
#1447 = FACE_OUTER_BOUND ( 'NONE', #829, .T. ) ;
#1448 = CARTESIAN_POINT ( 'NONE',  ( -10.12668159690567649, 1.256356190803088863E-15, -9.999999999999998224 ) ) ;
#1449 = CARTESIAN_POINT ( 'NONE',  ( -9.184850993605147944E-16, -28.37500000273118772, 5.000000000000000000 ) ) ;
#1450 = CARTESIAN_POINT ( 'NONE',  ( 4.391654775818395251, -2.390265326283149694, -3.125000000000002665 ) ) ;
#1451 = CARTESIAN_POINT ( 'NONE',  ( 3.152801135295366208, -28.56250000136559564, 3.152801135295367985 ) ) ;
#1452 =( NAMED_UNIT ( * ) PLANE_ANGLE_UNIT ( ) SI_UNIT ( $, .RADIAN. ) );
#1453 = ORIENTED_EDGE ( 'NONE', *, *, #10965, .T. ) ;
#1454 = CIRCLE ( 'NONE', #10504, 4.999999999999997335 ) ;
#1455 = ORIENTED_EDGE ( 'NONE', *, *, #15652, .F. ) ;
#1456 = PRODUCT_DEFINITION_SHAPE ( 'NONE', 'NONE',  #15978 ) ;
#1457 = VERTEX_POINT ( 'NONE', #5415 ) ;
#1458 = FACE_OUTER_BOUND ( 'NONE', #4862, .T. ) ;
#1459 = VECTOR ( 'NONE', #8668, 1000.000000000000114 ) ;
#1460 = EDGE_LOOP ( 'NONE', ( #15119, #13685, #4899, #13163 ) ) ;
#1461 = AXIS2_PLACEMENT_3D ( 'NONE', #4140, #2767, #5035 ) ;
#1462 = LINE ( 'NONE', #6485, #9231 ) ;
#1463 = ADVANCED_FACE ( 'NONE', ( #5722 ), #7027, .F. ) ;
#1464 = PRODUCT_RELATED_PRODUCT_CATEGORY ( 'part', '', ( #2282 ) ) ;
#1465 = AXIS2_PLACEMENT_3D ( 'NONE', #3196, #3040, #12886 ) ;
#1466 = CARTESIAN_POINT ( 'NONE',  ( 2.500000000000000000, -2.357898499370432610, 3.252606517456513302E-15 ) ) ;
#1467 = CARTESIAN_POINT ( 'NONE',  ( 1.846868145590736310, -30.87500000136559564, 4.458734124999999437 ) ) ;
#1468 = CARTESIAN_POINT ( 'NONE',  ( 4.458734124999999437, -26.50000000136559208, 1.846868145590737864 ) ) ;
#1469 = DIRECTION ( 'NONE',  ( -0.4999999999999918954, -6.123233995736766036E-17, 0.8660254037844432595 ) ) ;
#1470 = CARTESIAN_POINT ( 'NONE',  ( -3.033343224707664376, 3.753672977998667726, -4.249999998634406140 ) ) ;
#1471 = CARTESIAN_POINT ( 'NONE',  ( 67.49999999999931788, 40.00000000000000000, 2.081668171172168513E-14 ) ) ;
#1472 = DIRECTION ( 'NONE',  ( -0.000000000000000000, 1.000000000000000000, -0.000000000000000000 ) ) ;
#1473 = ORIENTED_EDGE ( 'NONE', *, *, #6665, .F. ) ;
#1474 = CARTESIAN_POINT ( 'NONE',  ( 4.474605093962741975, -3.763931520638213346, -48.59453411586688532 ) ) ;
#1475 =( LENGTH_UNIT ( ) NAMED_UNIT ( * ) SI_UNIT ( .MILLI., .METRE. ) );
#1476 = VERTEX_POINT ( 'NONE', #4588 ) ;
#1477 = CYLINDRICAL_SURFACE ( 'NONE', #2817, 10.00000000000000000 ) ;
#1478 = CIRCLE ( 'NONE', #4839, 60.00000000000000000 ) ;
#1479 = DIRECTION ( 'NONE',  ( -0.000000000000000000, 1.000000000000000000, -0.000000000000000000 ) ) ;
#1480 = ORIENTED_EDGE ( 'NONE', *, *, #10379, .T. ) ;
#1481 = CONTEXT_DEPENDENT_SHAPE_REPRESENTATION ( #5775, #12674 ) ;
#1482 = CARTESIAN_POINT ( 'NONE',  ( 3.916244202832140253, -2.131511515620588160, -6.687499998634407028 ) ) ;
#1483 = EDGE_CURVE ( 'NONE', #14678, #10126, #14455, .T. ) ;
#1484 = PRODUCT_DEFINITION ( 'UNKNOWN', '', #712, #8852 ) ;
#1485 = EDGE_CURVE ( 'NONE', #14775, #15211, #14382, .T. ) ;
#1486 = EDGE_CURVE ( 'NONE', #15428, #15685, #1262, .T. ) ;
#1487 = AXIS2_PLACEMENT_3D ( 'NONE', #13513, #11863, #2784 ) ;
#1488 = SURFACE_STYLE_USAGE ( .BOTH. , #7730 ) ;
#1489 =( BOUNDED_CURVE ( )  B_SPLINE_CURVE ( 2, ( #2657, #7609, #1450, #4196, #11466, #7779, #12749, #5423, #13805, #3955, #264 ),
 .UNSPECIFIED., .F., .F. ) 
 B_SPLINE_CURVE_WITH_KNOTS ( ( 3, 2, 2, 2, 2, 3 ),
 ( 0.5045872658012773293, 0.5124999999999999556, 0.5250000000000000222, 0.5374999999999999778, 0.5500000000000000444, 0.5545872658012773737 ),
 .UNSPECIFIED. ) 
 CURVE ( )  GEOMETRIC_REPRESENTATION_ITEM ( )  RATIONAL_B_SPLINE_CURVE ( ( 0.9646335149384803742, 0.9518143178943441196, 1.000000000000000000, 0.9238795325112867385, 1.000000000000000000, 0.9238795325112867385, 1.000000000000000000, 0.9238795325112867385, 1.000000000000000000, 0.9720652146169423968, 0.9646335149384803742 ) ) 
 REPRESENTATION_ITEM ( '' )  );
#1490 = PLANE ( 'NONE',  #2529 ) ;
#1491 = VECTOR ( 'NONE', #6393, 1000.000000000000000 ) ;
#1492 = DIRECTION ( 'NONE',  ( -0.5000000000000051070, 1.060575238724903217E-16, -0.8660254037844355990 ) ) ;
#1493 = AXIS2_PLACEMENT_3D ( 'NONE', #3815, #1630, #1554 ) ;
#1494 = CARTESIAN_POINT ( 'NONE',  ( 67.49999999999931788, 37.00000000000000000, -2.649999999999964828 ) ) ;
#1495 = CARTESIAN_POINT ( 'NONE',  ( -1.415196051561583790, 4.795541693661363958, -4.624999997268817609 ) ) ;
#1496 = CARTESIAN_POINT ( 'NONE',  ( -49.14213562373093680, -4.142135623730950122, 17.49999999999999645 ) ) ;
#1497 = PLANE ( 'NONE',  #14932 ) ;
#1498 = DIRECTION ( 'NONE',  ( -1.000000000000000000, 1.387778780781446464E-15, 0.000000000000000000 ) ) ;
#1499 = ORIENTED_EDGE ( 'NONE', *, *, #1640, .F. ) ;
#1500 = DIRECTION ( 'NONE',  ( 1.982541115402065110E-16, -1.000000000000000000, 0.000000000000000000 ) ) ;
#1501 = PLANE ( 'NONE',  #213 ) ;
#1502 = AXIS2_PLACEMENT_3D ( 'NONE', #3113, #6915, #14339 ) ;
#1503 = LINE ( 'NONE', #9031, #12792 ) ;
#1504 = ORIENTED_EDGE ( 'NONE', *, *, #13260, .T. ) ;
#1505 = ORIENTED_EDGE ( 'NONE', *, *, #8244, .F. ) ;
#1506 = VERTEX_POINT ( 'NONE', #15355 ) ;
#1507 = CARTESIAN_POINT ( 'NONE',  ( -4.795541693661363958, -1.415196051561583790, -0.5000000000000004441 ) ) ;
#1508 = CARTESIAN_POINT ( 'NONE',  ( -91.33974596215558961, -110.0591436588189254, 7.500000000000001776 ) ) ;
#1509 = ADVANCED_FACE ( 'NONE', ( #3066 ), #879, .F. ) ;
#1510 = CARTESIAN_POINT ( 'NONE',  ( 2.059999999999998721, 0.000000000000000000, -0.3080913168122742518 ) ) ;
#1511 = AXIS2_PLACEMENT_3D ( 'NONE', #4494, #9429, #860 ) ;
#1512 = AXIS2_PLACEMENT_3D ( 'NONE', #14485, #8045, #10457 ) ;
#1513 = CARTESIAN_POINT ( 'NONE',  ( 3.535533905932736864, -26.12500000000000355, 3.535533905932738641 ) ) ;
#1514 = CARTESIAN_POINT ( 'NONE',  ( -6.658902113225384944, -5.287118297634622266, -7.776713651266041971 ) ) ;
#1515 = FACE_OUTER_BOUND ( 'NONE', #7353, .T. ) ;
#1516 = CARTESIAN_POINT ( 'NONE',  ( 4.209348295687701302, 3.401574460001765665, -4.937500000000001776 ) ) ;
#1517 = CARTESIAN_POINT ( 'NONE',  ( 2.390265326283148806, 4.391654775818395251, -2.875000000000002665 ) ) ;
#1518 = VECTOR ( 'NONE', #3284, 1000.000000000000000 ) ;
#1519 = DIRECTION ( 'NONE',  ( 1.000000000000000000, 0.000000000000000000, 0.000000000000000000 ) ) ;
#1520 = CARTESIAN_POINT ( 'NONE',  ( 3.152801135295367541, -24.31250000136559564, -3.152801135295367541 ) ) ;
#1521 = AXIS2_PLACEMENT_3D ( 'NONE', #3947, #13886, #15033 ) ;
#1522 = CARTESIAN_POINT ( 'NONE',  ( -4.799145180956616130, 0.5093500532425063732, -5.124999998634405252 ) ) ;
#1523 = VERTEX_POINT ( 'NONE', #8254 ) ;
#1524 = CARTESIAN_POINT ( 'NONE',  ( -7.907996613752308335, -3.055722423191990611, -7.792112796859422374 ) ) ;
#1525 = ORIENTED_EDGE ( 'NONE', *, *, #6203, .T. ) ;
#1526 = EDGE_LOOP ( 'NONE', ( #5441, #6855, #1062, #15045 ) ) ;
#1527 = AXIS2_PLACEMENT_3D ( 'NONE', #7191, #12091, #1031 ) ;
#1528 = CARTESIAN_POINT ( 'NONE',  ( 4.458734124999999437, -21.50000000136559208, 1.846868145590737864 ) ) ;
#1529 = DIRECTION ( 'NONE',  ( -1.387778780781446464E-15, -1.000000000000000000, -0.000000000000000000 ) ) ;
#1530 = EDGE_LOOP ( 'NONE', ( #4141, #4262 ) ) ;
#1531 = LINE ( 'NONE', #13549, #15735 ) ;
#1532 = CARTESIAN_POINT ( 'NONE',  ( -1.261996585732579224, 4.276409079477648589, -1.062499998634405696 ) ) ;
#1533 = DIRECTION ( 'NONE',  ( -0.000000000000000000, -1.000000000000000000, -0.000000000000000000 ) ) ;
#1534 = CARTESIAN_POINT ( 'NONE',  ( 5.000000000000000000, -30.00000000000000000, 0.000000000000000000 ) ) ;
#1535 = CARTESIAN_POINT ( 'NONE',  ( -44.37834814142158280, -4.097106062772742696, -20.21050050139519172 ) ) ;
#1536 = CARTESIAN_POINT ( 'NONE',  ( 39.53738644056087992, 0.000000000000000000, -28.48076211352192999 ) ) ;
#1537 = CARTESIAN_POINT ( 'NONE',  ( 3.535533905932738197, -24.00000000273118772, -3.535533905932738197 ) ) ;
#1538 = DIRECTION ( 'NONE',  ( 0.000000000000000000, 0.000000000000000000, 1.000000000000000000 ) ) ;
#1539 = CARTESIAN_POINT ( 'NONE',  ( 3.152801135295367541, -31.31250000136559564, -3.152801135295367541 ) ) ;
#1540 = EDGE_CURVE ( 'NONE', #6438, #8156, #3851, .T. ) ;
#1541 = LINE ( 'NONE', #13807, #12251 ) ;
#1542 = ORIENTED_EDGE ( 'NONE', *, *, #3362, .T. ) ;
#1543 = ORIENTED_EDGE ( 'NONE', *, *, #6464, .F. ) ;
#1544 = PRESENTATION_STYLE_ASSIGNMENT (( #6858 ) ) ;
#1545 = ORIENTED_EDGE ( 'NONE', *, *, #13780, .F. ) ;
#1546 = DIRECTION ( 'NONE',  ( -0.000000000000000000, -0.000000000000000000, -1.000000000000000000 ) ) ;
#1547 = VERTEX_POINT ( 'NONE', #14221 ) ;
#1548 = CARTESIAN_POINT ( 'NONE',  ( 7.922281120364393914, -4.573931137438281169, -8.047472243342932430 ) ) ;
#1549 = CARTESIAN_POINT ( 'NONE',  ( -4.391654775818395251, 2.390265326283148806, -1.499999997268814500 ) ) ;
#1550 = CARTESIAN_POINT ( 'NONE',  ( 2.730187237215162345E-16, -30.43750000136559564, -4.458734124999999437 ) ) ;
#1551 = CARTESIAN_POINT ( 'NONE',  ( 5.000000000000095923, 0.7223674278660565662, -6.896799362785969834 ) ) ;
#1552 = CARTESIAN_POINT ( 'NONE',  ( 35.00000000000000000, 32.00000000000000000, 2.374647998151121317E-13 ) ) ;
#1553 = CARTESIAN_POINT ( 'NONE',  ( 1.261996585732578113, -4.276409079477644148, -4.812499998634405252 ) ) ;
#1554 = DIRECTION ( 'NONE',  ( 0.000000000000000000, 0.000000000000000000, 1.000000000000000000 ) ) ;
#1555 = ADVANCED_FACE ( 'NONE', ( #7105 ), #2081, .F. ) ;
#1557 = ADVANCED_FACE ( 'NONE', ( #1841 ), #4363, .F. ) ;
#1556 = ORIENTED_EDGE ( 'NONE', *, *, #13908, .T. ) ;
#1558 = CARTESIAN_POINT ( 'NONE',  ( 4.623788282402106375, -3.982459619753664803, -48.55488344125860323 ) ) ;
#1559 = VERTEX_POINT ( 'NONE', #8088 ) ;
#1560 = CARTESIAN_POINT ( 'NONE',  ( -114.4056415360013688, -110.1959696241292335, -17.50000000000000000 ) ) ;
#1561 = CARTESIAN_POINT ( 'NONE',  ( 4.458734124999999437, -31.43750000136559564, 0.000000000000000000 ) ) ;
#1562 = ORIENTED_EDGE ( 'NONE', *, *, #292, .T. ) ;
#1563 = CONTEXT_DEPENDENT_SHAPE_REPRESENTATION ( #12375, #1318 ) ;
#1564 = CARTESIAN_POINT ( 'NONE',  ( 4.799145180956616130, -0.5093500532425063732, -5.624999998634405252 ) ) ;
#1565 = CARTESIAN_POINT ( 'NONE',  ( 2.100000000000000089, 0.000000000000000000, -0.2800830152838844622 ) ) ;
#1566 = DIRECTION ( 'NONE',  ( 0.8660254037844379305, 0.5000000000000013323, 0.000000000000000000 ) ) ;
#1567 = CARTESIAN_POINT ( 'NONE',  ( 2.500000000000000000, 2.500728763858895382E-16, -2.041999999999999815 ) ) ;
#1568 = CYLINDRICAL_SURFACE ( 'NONE', #10807, 5.000000000000000000 ) ;
#1569 = CARTESIAN_POINT ( 'NONE',  ( 2.390265326283148806, 4.391654775818395251, -4.749999997268817609 ) ) ;
#1570 = CARTESIAN_POINT ( 'NONE',  ( -55.00000000000000000, -10.00000000000000178, 17.50000000000000000 ) ) ;
#1571 = EDGE_CURVE ( 'NONE', #10747, #11884, #6000, .T. ) ;
#1572 = CARTESIAN_POINT ( 'NONE',  ( -4.662267971122446397, 0.3223875400172048211, -0.2364825125149292995 ) ) ;
#1573 = CARTESIAN_POINT ( 'NONE',  ( -35.00000000000000000, 37.00000000000000000, 6.000000000000000000 ) ) ;
#1574 = EDGE_CURVE ( 'NONE', #13609, #12993, #6074, .T. ) ;
#1575 = ORIENTED_EDGE ( 'NONE', *, *, #762, .F. ) ;
#1576 = DIRECTION ( 'NONE',  ( 0.000000000000000000, -0.000000000000000000, 1.000000000000000000 ) ) ;
#1577 = CARTESIAN_POINT ( 'NONE',  ( -4.197393957002303999, -7.773935952363655451E-14, -3.503767560748929810 ) ) ;
#1578 = ORIENTED_EDGE ( 'NONE', *, *, #15530, .F. ) ;
#1579 = ORIENTED_EDGE ( 'NONE', *, *, #8085, .F. ) ;
#1580 = VERTEX_POINT ( 'NONE', #955 ) ;
#1581 = CARTESIAN_POINT ( 'NONE',  ( -0.5711823568785977523, -5.381735091635034607, -0.3124999999999993339 ) ) ;
#1582 = PLANE ( 'NONE',  #15664 ) ;
#1583 =( BOUNDED_CURVE ( )  B_SPLINE_CURVE ( 2, ( #3767, #3854, #1513, #12646, #4002, #12480, #10084, #15011, #14935 ),
 .UNSPECIFIED., .F., .F. ) 
 B_SPLINE_CURVE_WITH_KNOTS ( ( 3, 2, 2, 2, 3 ),
 ( 0.5749999999999998446, 0.5874999999999999112, 0.5999999999999998668, 0.6124999999999999334, 0.6249999999999998890 ),
 .UNSPECIFIED. ) 
 CURVE ( )  GEOMETRIC_REPRESENTATION_ITEM ( )  RATIONAL_B_SPLINE_CURVE ( ( 1.000000000000000666, 0.9238795325112860723, 1.000000000000000000, 0.9238795325112867385, 1.000000000000000000, 0.9238795325112867385, 1.000000000000000000, 0.9238795325112874046, 0.9999999999999993339 ) ) 
 REPRESENTATION_ITEM ( '' )  );
#1584 = LINE ( 'NONE', #12719, #11976 ) ;
#1585 = CARTESIAN_POINT ( 'NONE',  ( -2.621086668468696868, -7.606368536631369359, -7.634085501268423890 ) ) ;
#1586 = CARTESIAN_POINT ( 'NONE',  ( -6.250000000000015987, 5.051814855409245020, -7.198902722707438251 ) ) ;
#1587 = CARTESIAN_POINT ( 'NONE',  ( -44.99999999999999289, -11.00000000000000178, -3.999999999999170885 ) ) ;
#1588 = CARTESIAN_POINT ( 'NONE',  ( 4.209348295687701302, 3.401574460001765665, -5.937500000000002665 ) ) ;
#1589 = CARTESIAN_POINT ( 'NONE',  ( -49.14213562373093680, -30.85786437626904899, -17.49999999999999645 ) ) ;
#1590 = CIRCLE ( 'NONE', #826, 2.649999999999985700 ) ;
#1591 = CARTESIAN_POINT ( 'NONE',  ( 2.071067811865482611, -28.81250000000000000, -4.999999999999992895 ) ) ;
#1592 = CARTESIAN_POINT ( 'NONE',  ( -4.458734125000000326, -24.00000000136559564, -1.846868145590735644 ) ) ;
#1593 = EDGE_CURVE ( 'NONE', #2810, #7938, #11124, .T. ) ;
#1594 = CARTESIAN_POINT ( 'NONE',  ( 3.033343224707661712, -3.753672977998669946, -5.749999998634407916 ) ) ;
#1595 = ORIENTED_EDGE ( 'NONE', *, *, #11836, .F. ) ;
#1596 = CARTESIAN_POINT ( 'NONE',  ( 3.749999999999999112, 6.495190528383289141, -6.991905250253754645 ) ) ;
#1597 = VERTEX_POINT ( 'NONE', #11053 ) ;
#1598 = ORIENTED_EDGE ( 'NONE', *, *, #8419, .T. ) ;
#1599 = CARTESIAN_POINT ( 'NONE',  ( 4.458734125000000326, -22.37500000136559564, -1.846868145590734978 ) ) ;
#1600 = CARTESIAN_POINT ( 'NONE',  ( -55.00000000000000000, 0.000000000000000000, -18.00000000000001066 ) ) ;
#1601 = VERTEX_POINT ( 'NONE', #1178 ) ;
#1602 = CARTESIAN_POINT ( 'NONE',  ( -3.535533905932738641, -28.37500000000000000, 3.535533905932737309 ) ) ;
#1603 = LINE ( 'NONE', #168, #7207 ) ;
#1604 = DIRECTION ( 'NONE',  ( 0.000000000000000000, 0.000000000000000000, -1.000000000000000000 ) ) ;
#1605 = CARTESIAN_POINT ( 'NONE',  ( 2.500000000000000000, 2.357898499370433054, -1.951563910473907981E-15 ) ) ;
#1606 = CARTESIAN_POINT ( 'NONE',  ( 5.000000000000000000, -28.06250000000000000, 2.071067811865478614 ) ) ;
#1607 = LINE ( 'NONE', #6632, #11168 ) ;
#1608 = CARTESIAN_POINT ( 'NONE',  ( 2.500000000000000000, 1.178949249685218525, 2.041999999999999371 ) ) ;
#1609 = CARTESIAN_POINT ( 'NONE',  ( 3.535533905932736864, -25.25000000273118417, 3.535533905932738641 ) ) ;
#1610 = EDGE_CURVE ( 'NONE', #10210, #14193, #2463, .T. ) ;
#1611 = FACE_BOUND ( 'NONE', #4354, .T. ) ;
#1612 = CARTESIAN_POINT ( 'NONE',  ( 3.152801135295366208, -27.56250000136559564, 3.152801135295367985 ) ) ;
#1613 = CARTESIAN_POINT ( 'NONE',  ( 2.100000000000000089, 0.000000000000000000, -5.000000000000000000 ) ) ;
#1614 = ORIENTED_EDGE ( 'NONE', *, *, #11960, .F. ) ;
#1615 = ORIENTED_EDGE ( 'NONE', *, *, #3613, .F. ) ;
#1616 = AXIS2_PLACEMENT_3D ( 'NONE', #5338, #10277, #15205 ) ;
#1617 = ORIENTED_EDGE ( 'NONE', *, *, #5827, .F. ) ;
#1618 = AXIS2_PLACEMENT_3D ( 'NONE', #10717, #15416, #6844 ) ;
#1619 = LINE ( 'NONE', #5103, #7647 ) ;
#1620 = ORIENTED_EDGE ( 'NONE', *, *, #9961, .F. ) ;
#1621 = DIRECTION ( 'NONE',  ( 0.000000000000000000, 0.000000000000000000, 1.000000000000000000 ) ) ;
#1622 = EDGE_CURVE ( 'NONE', #10806, #15506, #12697, .T. ) ;
#1623 = EDGE_CURVE ( 'NONE', #14249, #8765, #15046, .T. ) ;
#1624 = CARTESIAN_POINT ( 'NONE',  ( -6.765421556309547668E-13, 40.00000000000000000, 67.49999999999930367 ) ) ;
#1625 = CARTESIAN_POINT ( 'NONE',  ( 4.458734124999999437, -30.68750000136559564, 0.000000000000000000 ) ) ;
#1626 = AXIS2_PLACEMENT_3D ( 'NONE', #8984, #1538, #6552 ) ;
#1627 = CARTESIAN_POINT ( 'NONE',  ( 0.5711823568785988625, 5.381735091635026613, -5.812500000000000000 ) ) ;
#1628 = VECTOR ( 'NONE', #11144, 1000.000000000000000 ) ;
#1629 = DIRECTION ( 'NONE',  ( 1.000000000000000000, 0.000000000000000000, 0.000000000000000000 ) ) ;
#1630 = DIRECTION ( 'NONE',  ( 0.000000000000000000, 1.000000000000000000, 0.000000000000000000 ) ) ;
#1631 = ORIENTED_EDGE ( 'NONE', *, *, #15956, .F. ) ;
#1632 = B_SPLINE_CURVE_WITH_KNOTS ( 'NONE', 3,
 ( #4131, #5190, #13910, #11635, #6410, #3965 ),
 .UNSPECIFIED., .F., .F.,
 ( 4, 2, 4 ),
 ( 0.000000000000000000, 0.002307655110370372166, 0.004615310220740744332 ),
 .UNSPECIFIED. ) ;
#1633 = VERTEX_POINT ( 'NONE', #4983 ) ;
#1634 = CARTESIAN_POINT ( 'NONE',  ( -21.01110699893060030, -3.000000000000000000, 39.04230484541323420 ) ) ;
#1635 = DIRECTION ( 'NONE',  ( -0.000000000000000000, -1.000000000000000000, -0.000000000000000000 ) ) ;
#1636 = ORIENTED_EDGE ( 'NONE', *, *, #9965, .T. ) ;
#1637 = CARTESIAN_POINT ( 'NONE',  ( -3.033343224707664820, 3.753672977998667726, -6.249999998634408804 ) ) ;
#1638 = FACE_OUTER_BOUND ( 'NONE', #14267, .T. ) ;
#1639 = EDGE_CURVE ( 'NONE', #2543, #5402, #1357, .T. ) ;
#1640 = EDGE_CURVE ( 'NONE', #15020, #3371, #4274, .T. ) ;
#1641 = CARTESIAN_POINT ( 'NONE',  ( -2.390265326283148806, -4.391654775818394363, -5.249999997268817609 ) ) ;
#1642 = CARTESIAN_POINT ( 'NONE',  ( 1.415196051561583790, -4.795541693661363958, -8.124999997268814056 ) ) ;
#1643 = CARTESIAN_POINT ( 'NONE',  ( -4.209348295687703967, -3.401574460001763001, -4.312499997268816720 ) ) ;
#1644 = LINE ( 'NONE', #11268, #8249 ) ;
#1645 = DIRECTION ( 'NONE',  ( 0.000000000000000000, 0.000000000000000000, -1.000000000000000000 ) ) ;
#1646 = CARTESIAN_POINT ( 'NONE',  ( -8.190561711645485556E-16, -21.93750000136559208, 4.458734124999999437 ) ) ;
#1647 = ORIENTED_EDGE ( 'NONE', *, *, #7708, .F. ) ;
#1648 = DIRECTION ( 'NONE',  ( 0.000000000000000000, 1.000000000000000000, 0.000000000000000000 ) ) ;
#1649 = CARTESIAN_POINT ( 'NONE',  ( -116.3391301858327296, -120.2076149402627294, 7.500000000000001776 ) ) ;
#1650 = CARTESIAN_POINT ( 'NONE',  ( 0.000000000000000000, -13.00000000000000178, 0.000000000000000000 ) ) ;
#1651 = VERTEX_POINT ( 'NONE', #5883 ) ;
#1652 = DIRECTION ( 'NONE',  ( 0.000000000000000000, 0.000000000000000000, 1.000000000000000000 ) ) ;
#1653 = ORIENTED_EDGE ( 'NONE', *, *, #7005, .F. ) ;
#1654 = VERTEX_POINT ( 'NONE', #7262 ) ;
#1655 = DIRECTION ( 'NONE',  ( -0.000000000000000000, 1.000000000000000000, -0.000000000000000000 ) ) ;
#1656 = CARTESIAN_POINT ( 'NONE',  ( -0.5276280594146446346, 4.314175951381965746, -3.320322319201721495 ) ) ;
#1657 = FACE_OUTER_BOUND ( 'NONE', #13410, .T. ) ;
#1658 = ADVANCED_FACE ( 'NONE', ( #2550, #7189, #4907, #6041, #9667, #3612, #13379 ), #15756, .T. ) ;
#1659 = AXIS2_PLACEMENT_3D ( 'NONE', #8626, #6359, #3760 ) ;
#1660 = FACE_OUTER_BOUND ( 'NONE', #1712, .T. ) ;
#1661 = FACE_OUTER_BOUND ( 'NONE', #5077, .T. ) ;
#1662 = AXIS2_PLACEMENT_3D ( 'NONE', #13941, #5063, #2795 ) ;
#1663 = DIRECTION ( 'NONE',  ( 0.000000000000000000, -0.000000000000000000, 1.000000000000000000 ) ) ;
#1664 = CARTESIAN_POINT ( 'NONE',  ( -4.391654775818395251, 2.390265326283148806, -4.625000000000000888 ) ) ;
#1665 = DIRECTION ( 'NONE',  ( -1.000000000000000000, -0.000000000000000000, -0.000000000000000000 ) ) ;
#1666 = CARTESIAN_POINT ( 'NONE',  ( -2.742827927723112236, -3.035229711105190464, -3.433252694550595230 ) ) ;
#1667 = CARTESIAN_POINT ( 'NONE',  ( 0.000000000000000000, -20.00000000000000000, 0.000000000000000000 ) ) ;
#1668 = CARTESIAN_POINT ( 'NONE',  ( -2.131511515620587272, -3.916244202832140253, -6.937499998634407916 ) ) ;
#1669 = EDGE_LOOP ( 'NONE', ( #11062, #5715, #3885, #9341 ) ) ;
#1670 = CARTESIAN_POINT ( 'NONE',  ( 4.999999999999999112, 5.773502691896254646, -7.063244554130000630 ) ) ;
#1671 = ORIENTED_EDGE ( 'NONE', *, *, #6597, .T. ) ;
#1672 = VERTEX_POINT ( 'NONE', #8479 ) ;
#1673 =( GEOMETRIC_REPRESENTATION_CONTEXT ( 3 ) GLOBAL_UNCERTAINTY_ASSIGNED_CONTEXT ( ( #6941 ) ) GLOBAL_UNIT_ASSIGNED_CONTEXT ( ( #8215, #13115, #691 ) ) REPRESENTATION_CONTEXT ( 'NONE', 'WORKASPACE' ) );
#1674 =( BOUNDED_SURFACE ( )  B_SPLINE_SURFACE ( 1, 2, ( 
 ( #1561, #10216, #8769, #204, #6572, #5365, #11411, #2845, #436, #7800, #10304, #2095, #8269, #13306, #4601, #8338, #2249, #2020, #3009, #7040, #12771, #9681, #11574, #14540, #895, #11941, #7119, #5898, #7958, #9164, #10827, #5815, #12020, #3319, #3389, #15769, #13161, #7203, #1042, #10750, #2169, #12860, #8415, #10377, #970, #2923, #5735, #4524, #4680, #15687, #4221, #15841, #13230, #10673, #815, #1716, #14082, #528, #9539, #6968, #7873, #15605, #6664, #3459, #9604, #12104, #14467, #10900, #15305, #5444, #5977, #11869, #9458, #4759, #14390, #3700, #8730, #6140, #13392, #13458, #11138, #6301, #13635, #11067, #77, #6381, #1353, #11216, #163, #12419, #2645, #3784, #6055, #2399, #7350, #12175, #14862, #14704, #2563, #1277, #7516, #12257, #4843, #5080, #3626, #1115, #10014, #4, #3868, #11300, #3539, #4995, #8807, #9922, #7596, #12494, #1435, #7274, #14952, #8570, #13711, #252, #5168, #1196, #14619, #8496, #2330, #10982, #15922, #9769, #4920, #12342, #9846, #14777, #6224, #8646, #13543, #2477, #7437, #7768, #4018, #6778, #6537, #10342, #12659, #1599, #8887, #328, #2725, #11533, #15099, #639, #11452, #15024, #10412, #15269, #11611, #485, #1833, #1528, #10097 ),
 ( #15188, #4183, #399, #13789, #8968, #6619, #1762, #9129, #5324, #5407, #11687, #12816, #6709, #562, #7916, #14129, #14040, #6465, #13879, #2812, #7680, #2966, #10174, #5483, #12734, #15348, #10263, #5237, #4266, #4104, #12579, #9208, #9053, #3058, #3939, #11377, #8004, #12901, #13956, #2889, #7840, #1676, #14215, #2076, #15512, #2150, #13209, #8320, #9362, #14520, #9588, #15751, #7099, #4581, #8393, #719, #3295, #7021, #5645, #8247, #10586, #11767, #11923, #11849, #3209, #4429, #2227, #1997, #10729, #4664, #14287, #8158, #9439, #15432, #12082, #3135, #950, #13143, #4502, #9519, #12000, #13059, #6947, #5877, #14366, #14451, #5716, #5792, #10811, #10654, #3440, #13286, #15586, #3373, #796, #7181, #12977, #5564, #10500, #875, #15667, #4352, #9290, #6860, #8081, #1913, #1173, #139, #4903, #6037, #6115, #6119, #11194, #2458, #2382, #14841, #11045, #8473, #7258, #14685, #13612, #3606, #12158, #12235, #5059, #14929, #7415, #9995, #13374, #11121, #9828, #3849, #3519, #1026, #1096, #10957, #60, #4975, #2544, #12400, #14758, #8553, #3763, #13522, #3681, #2313, #10881, #15901, #12319, #8790, #13693, #4820, #4740, #9747, #13442, #2627, #1258, #14596, #7578, #8709, #8628 ) ),
 .UNSPECIFIED., .F., .F., .F. ) 
 B_SPLINE_SURFACE_WITH_KNOTS ( ( 2, 2 ),
 ( 3, 2, 2, 2, 2, 2, 2, 2, 2, 2, 2, 2, 2, 2, 2, 2, 2, 2, 2, 2, 2, 2, 2, 2, 2, 2, 2, 2, 2, 2, 2, 2, 2, 2, 2, 2, 2, 2, 2, 2, 2, 2, 2, 2, 2, 2, 2, 2, 2, 2, 2, 2, 2, 2, 2, 2, 2, 2, 2, 2, 2, 2, 2, 2, 2, 2, 2, 2, 2, 2, 2, 2, 2, 2, 2, 2, 2, 2, 2, 2, 3 ),
 ( 0.000000000000000000, 1.000000000000000000 ),
 ( 0.000000000000000000, 0.01250000000000000069, 0.02500000000000000139, 0.03749999999999999861, 0.05000000000000000278, 0.06250000000000000000, 0.07499999999999999722, 0.08749999999999999445, 0.1000000000000000056, 0.1125000000000000028, 0.1250000000000000000, 0.1375000000000000111, 0.1499999999999999944, 0.1625000000000000056, 0.1749999999999999889, 0.1875000000000000000, 0.2000000000000000111, 0.2124999999999999944, 0.2250000000000000056, 0.2374999999999999889, 0.2500000000000000000, 0.2625000000000000111, 0.2750000000000000222, 0.2874999999999999778, 0.2999999999999999889, 0.3125000000000000000, 0.3250000000000000111, 0.3375000000000000222, 0.3499999999999999778, 0.3624999999999999889, 0.3750000000000000000, 0.3875000000000000111, 0.4000000000000000222, 0.4124999999999999778, 0.4249999999999999889, 0.4375000000000000000, 0.4500000000000000111, 0.4625000000000000222, 0.4749999999999999778, 0.4874999999999999889, 0.5000000000000000000, 0.5124999999999999556, 0.5250000000000000222, 0.5374999999999999778, 0.5500000000000000444, 0.5625000000000000000, 0.5749999999999999556, 0.5875000000000000222, 0.5999999999999999778, 0.6125000000000000444, 0.6250000000000000000, 0.6374999999999999556, 0.6500000000000000222, 0.6624999999999999778, 0.6750000000000000444, 0.6875000000000000000, 0.6999999999999999556, 0.7125000000000000222, 0.7249999999999999778, 0.7375000000000000444, 0.7500000000000000000, 0.7624999999999999556, 0.7750000000000000222, 0.7874999999999999778, 0.8000000000000000444, 0.8125000000000000000, 0.8249999999999999556, 0.8375000000000000222, 0.8499999999999999778, 0.8625000000000000444, 0.8750000000000000000, 0.8874999999999999556, 0.9000000000000000222, 0.9124999999999999778, 0.9250000000000000444, 0.9375000000000000000, 0.9499999999999999556, 0.9625000000000000222, 0.9749999999999999778, 0.9875000000000000444, 1.000000000000000000 ),
 .UNSPECIFIED. ) 
 GEOMETRIC_REPRESENTATION_ITEM ( )  RATIONAL_B_SPLINE_SURFACE ( (
 ( 1.000000000000000000, 0.9238795325112867385, 1.000000000000000000, 0.9238795325112867385, 1.000000000000000000, 0.9238795325112867385, 1.000000000000000000, 0.9238795325112867385, 1.000000000000000000, 0.9238795325112867385, 1.000000000000000000, 0.9238795325112867385, 1.000000000000000000, 0.9238795325112867385, 1.000000000000000000, 0.9238795325112867385, 1.000000000000000000, 0.9238795325112867385, 1.000000000000000000, 0.9238795325112867385, 1.000000000000000000, 0.9238795325112867385, 1.000000000000000000, 0.9238795325112867385, 1.000000000000000000, 0.9238795325112867385, 1.000000000000000000, 0.9238795325112867385, 1.000000000000000000, 0.9238795325112867385, 1.000000000000000000, 0.9238795325112867385, 1.000000000000000000, 0.9238795325112867385, 1.000000000000000000, 0.9238795325112867385, 1.000000000000000000, 0.9238795325112867385, 1.000000000000000000, 0.9238795325112867385, 1.000000000000000000, 0.9238795325112867385, 1.000000000000000000, 0.9238795325112867385, 1.000000000000000000, 0.9238795325112867385, 1.000000000000000000, 0.9238795325112867385, 1.000000000000000000, 0.9238795325112867385, 1.000000000000000000, 0.9238795325112867385, 1.000000000000000000, 0.9238795325112867385, 1.000000000000000000, 0.9238795325112867385, 1.000000000000000000, 0.9238795325112867385, 1.000000000000000000, 0.9238795325112867385, 1.000000000000000000, 0.9238795325112867385, 1.000000000000000000, 0.9238795325112867385, 1.000000000000000000, 0.9238795325112867385, 1.000000000000000000, 0.9238795325112867385, 1.000000000000000000, 0.9238795325112867385, 1.000000000000000000, 0.9238795325112867385, 1.000000000000000000, 0.9238795325112867385, 1.000000000000000000, 0.9238795325112867385, 1.000000000000000000, 0.9238795325112867385, 1.000000000000000000, 0.9238795325112867385, 1.000000000000000000, 0.9238795325112867385, 1.000000000000000000, 0.9238795325112867385, 1.000000000000000000, 0.9238795325112867385, 1.000000000000000000, 0.9238795325112867385, 1.000000000000000000, 0.9238795325112867385, 1.000000000000000000, 0.9238795325112867385, 1.000000000000000000, 0.9238795325112867385, 1.000000000000000000, 0.9238795325112867385, 1.000000000000000000, 0.9238795325112867385, 1.000000000000000000, 0.9238795325112867385, 1.000000000000000000, 0.9238795325112867385, 1.000000000000000000, 0.9238795325112867385, 1.000000000000000000, 0.9238795325112867385, 1.000000000000000000, 0.9238795325112867385, 1.000000000000000000, 0.9238795325112867385, 1.000000000000000000, 0.9238795325112867385, 1.000000000000000000, 0.9238795325112867385, 1.000000000000000000, 0.9238795325112867385, 1.000000000000000000, 0.9238795325112867385, 1.000000000000000000, 0.9238795325112867385, 1.000000000000000000, 0.9238795325112867385, 1.000000000000000000, 0.9238795325112867385, 1.000000000000000000, 0.9238795325112867385, 1.000000000000000000, 0.9238795325112867385, 1.000000000000000000, 0.9238795325112867385, 1.000000000000000000, 0.9238795325112867385, 1.000000000000000000, 0.9238795325112867385, 1.000000000000000000, 0.9238795325112867385, 1.000000000000000000, 0.9238795325112867385, 1.000000000000000000, 0.9238795325112867385, 1.000000000000000000, 0.9238795325112867385, 1.000000000000000000, 0.9238795325112867385, 1.000000000000000000, 0.9238795325112867385, 1.000000000000000000, 0.9238795325112867385, 1.000000000000000000, 0.9238795325112867385, 1.000000000000000000, 0.9238795325112867385, 1.000000000000000000, 0.9238795325112867385, 1.000000000000000000, 0.9238795325112867385, 1.000000000000000000, 0.9238795325112867385, 1.000000000000000000, 0.9238795325112867385, 1.000000000000000000),
 ( 1.000000000000000000, 0.9238795325112867385, 1.000000000000000000, 0.9238795325112867385, 1.000000000000000000, 0.9238795325112867385, 1.000000000000000000, 0.9238795325112867385, 1.000000000000000000, 0.9238795325112867385, 1.000000000000000000, 0.9238795325112867385, 1.000000000000000000, 0.9238795325112867385, 1.000000000000000000, 0.9238795325112867385, 1.000000000000000000, 0.9238795325112867385, 1.000000000000000000, 0.9238795325112867385, 1.000000000000000000, 0.9238795325112867385, 1.000000000000000000, 0.9238795325112867385, 1.000000000000000000, 0.9238795325112867385, 1.000000000000000000, 0.9238795325112867385, 1.000000000000000000, 0.9238795325112867385, 1.000000000000000000, 0.9238795325112867385, 1.000000000000000000, 0.9238795325112867385, 1.000000000000000000, 0.9238795325112867385, 1.000000000000000000, 0.9238795325112867385, 1.000000000000000000, 0.9238795325112867385, 1.000000000000000000, 0.9238795325112867385, 1.000000000000000000, 0.9238795325112867385, 1.000000000000000000, 0.9238795325112867385, 1.000000000000000000, 0.9238795325112867385, 1.000000000000000000, 0.9238795325112867385, 1.000000000000000000, 0.9238795325112867385, 1.000000000000000000, 0.9238795325112867385, 1.000000000000000000, 0.9238795325112867385, 1.000000000000000000, 0.9238795325112867385, 1.000000000000000000, 0.9238795325112867385, 1.000000000000000000, 0.9238795325112867385, 1.000000000000000000, 0.9238795325112867385, 1.000000000000000000, 0.9238795325112867385, 1.000000000000000000, 0.9238795325112867385, 1.000000000000000000, 0.9238795325112867385, 1.000000000000000000, 0.9238795325112867385, 1.000000000000000000, 0.9238795325112867385, 1.000000000000000000, 0.9238795325112867385, 1.000000000000000000, 0.9238795325112867385, 1.000000000000000000, 0.9238795325112867385, 1.000000000000000000, 0.9238795325112867385, 1.000000000000000000, 0.9238795325112867385, 1.000000000000000000, 0.9238795325112867385, 1.000000000000000000, 0.9238795325112867385, 1.000000000000000000, 0.9238795325112867385, 1.000000000000000000, 0.9238795325112867385, 1.000000000000000000, 0.9238795325112867385, 1.000000000000000000, 0.9238795325112867385, 1.000000000000000000, 0.9238795325112867385, 1.000000000000000000, 0.9238795325112867385, 1.000000000000000000, 0.9238795325112867385, 1.000000000000000000, 0.9238795325112867385, 1.000000000000000000, 0.9238795325112867385, 1.000000000000000000, 0.9238795325112867385, 1.000000000000000000, 0.9238795325112867385, 1.000000000000000000, 0.9238795325112867385, 1.000000000000000000, 0.9238795325112867385, 1.000000000000000000, 0.9238795325112867385, 1.000000000000000000, 0.9238795325112867385, 1.000000000000000000, 0.9238795325112867385, 1.000000000000000000, 0.9238795325112867385, 1.000000000000000000, 0.9238795325112867385, 1.000000000000000000, 0.9238795325112867385, 1.000000000000000000, 0.9238795325112867385, 1.000000000000000000, 0.9238795325112867385, 1.000000000000000000, 0.9238795325112867385, 1.000000000000000000, 0.9238795325112867385, 1.000000000000000000, 0.9238795325112867385, 1.000000000000000000, 0.9238795325112867385, 1.000000000000000000, 0.9238795325112867385, 1.000000000000000000, 0.9238795325112867385, 1.000000000000000000, 0.9238795325112867385, 1.000000000000000000, 0.9238795325112867385, 1.000000000000000000, 0.9238795325112867385, 1.000000000000000000, 0.9238795325112867385, 1.000000000000000000, 0.9238795325112867385, 1.000000000000000000, 0.9238795325112867385, 1.000000000000000000, 0.9238795325112867385, 1.000000000000000000, 0.9238795325112867385, 1.000000000000000000, 0.9238795325112867385, 1.000000000000000000) ) ) 
 REPRESENTATION_ITEM ( '' )  SURFACE ( )  );
#1675 = VERTEX_POINT ( 'NONE', #13291 ) ;
#1676 = CARTESIAN_POINT ( 'NONE',  ( -4.458734125000001214, -29.12500000136559919, 1.846868145590734089 ) ) ;
#1677 = CARTESIAN_POINT ( 'NONE',  ( -41.99999999999978684, -11.00000000000000178, 1.499999999999999112 ) ) ;
#1678 = AXIS2_PLACEMENT_3D ( 'NONE', #4647, #9572, #6017 ) ;
#1679 = ORIENTED_EDGE ( 'NONE', *, *, #6309, .F. ) ;
#1680 = DIRECTION ( 'NONE',  ( 0.000000000000000000, 0.000000000000000000, 1.000000000000000000 ) ) ;
#1681 = ADVANCED_FACE ( 'NONE', ( #12088 ), #2318, .F. ) ;
#1682 = ADVANCED_FACE ( 'NONE', ( #10964 ), #2635, .T. ) ;
#1683 = EDGE_CURVE ( 'NONE', #13499, #13973, #4204, .T. ) ;
#1684 = EDGE_CURVE ( 'NONE', #4500, #5972, #13528, .T. ) ;
#1685 = CARTESIAN_POINT ( 'NONE',  ( 7.499999999998624212, 3.882635837268421763, -7.781684861373589612 ) ) ;
#1686 = CARTESIAN_POINT ( 'NONE',  ( 4.799145180956616130, -0.5093500532425063732, -2.374999998634407028 ) ) ;
#1687 = CYLINDRICAL_SURFACE ( 'NONE', #11678, 2.500000000000909495 ) ;
#1688 = CARTESIAN_POINT ( 'NONE',  ( 2.071067811865476394, -29.18750000000000711, 5.000000000000000000 ) ) ;
#1689 = AXIS2_PLACEMENT_3D ( 'NONE', #3622, #7512, #12252 ) ;
#1690 = CARTESIAN_POINT ( 'NONE',  ( 4.799145180956616130, -0.5093500532425063732, -5.374999998634406140 ) ) ;
#1691 = CARTESIAN_POINT ( 'NONE',  ( -2.071067811865447084, -21.81250000273119483, -5.000000000000029310 ) ) ;
#1692 = FACE_OUTER_BOUND ( 'NONE', #5404, .T. ) ;
#1693 = CARTESIAN_POINT ( 'NONE',  ( -3.535533905932737309, -25.75000000273118417, -3.535533905932738197 ) ) ;
#1694 = DIRECTION ( 'NONE',  ( -0.000000000000000000, -1.000000000000000000, -0.000000000000000000 ) ) ;
#1695 = CARTESIAN_POINT ( 'NONE',  ( -8.190561711645485556E-16, -27.68750000136559564, 4.458734124999999437 ) ) ;
#1696 = CARTESIAN_POINT ( 'NONE',  ( 4.599534470798633201, -6.460478697736662390, -7.590212325761508616 ) ) ;
#1697 = ORIENTED_EDGE ( 'NONE', *, *, #4108, .T. ) ;
#1698 = VERTEX_POINT ( 'NONE', #7421 ) ;
#1699 = ORIENTED_EDGE ( 'NONE', *, *, #14620, .T. ) ;
#1700 = CARTESIAN_POINT ( 'NONE',  ( -44.32140357639302408, -3.763931520639085093, 20.42214537465778790 ) ) ;
#1701 = CIRCLE ( 'NONE', #14866, 4.000000000000000000 ) ;
#1702 = ORIENTED_EDGE ( 'NONE', *, *, #2061, .F. ) ;
#1703 = CARTESIAN_POINT ( 'NONE',  ( 7.897850199329718990, -1.533397866934080644, -7.634054012537967004 ) ) ;
#1704 = VECTOR ( 'NONE', #6466, 1000.000000000000000 ) ;
#1705 = ADVANCED_FACE ( 'NONE', ( #12327 ), #8721, .F. ) ;
#1706 = CARTESIAN_POINT ( 'NONE',  ( -28.86751345948145442, 1.999999999999994893, -18.00000000000001066 ) ) ;
#1707 = DIRECTION ( 'NONE',  ( 0.000000000000000000, 0.000000000000000000, 1.000000000000000000 ) ) ;
#1708 = CARTESIAN_POINT ( 'NONE',  ( 12.67949192431126093, -37.00000000000000711, -61.96152422706632024 ) ) ;
#1709 = AXIS2_PLACEMENT_3D ( 'NONE', #7658, #12787, #5294 ) ;
#1710 = CARTESIAN_POINT ( 'NONE',  ( 3.916244202832140253, -2.131511515620588160, -7.687499998634407916 ) ) ;
#1711 = CARTESIAN_POINT ( 'NONE',  ( 35.00000000000000000, 50.00000000000000000, 2.649999999999992806 ) ) ;
#1712 = EDGE_LOOP ( 'NONE', ( #11511, #6827, #8550, #14364 ) ) ;
#1713 = CIRCLE ( 'NONE', #1979, 57.99999999999999289 ) ;
#1714 = ORIENTED_EDGE ( 'NONE', *, *, #120, .T. ) ;
#1715 = DIRECTION ( 'NONE',  ( -0.000000000000000000, -1.000000000000000000, -0.000000000000000000 ) ) ;
#1716 = CARTESIAN_POINT ( 'NONE',  ( -4.458734125000000326, -28.00000000136559564, -1.846868145590735644 ) ) ;
#1717 = EDGE_LOOP ( 'NONE', ( #3204, #14325, #8748, #11994 ) ) ;
#1718 = AXIS2_PLACEMENT_3D ( 'NONE', #2231, #7261, #4667 ) ;
#1719 = CARTESIAN_POINT ( 'NONE',  ( 5.000000000000004441, 3.034671531081452754E-15, -0.04526304759294640795 ) ) ;
#1720 = LINE ( 'NONE', #7962, #13361 ) ;
#1721 = CARTESIAN_POINT ( 'NONE',  ( -2.688821387764050996E-14, -4.618802153517012954, -0.4999999999999995559 ) ) ;
#1722 = UNCERTAINTY_MEASURE_WITH_UNIT (LENGTH_MEASURE( 1.000000000000000082E-05 ), #14214, 'distance_accuracy_value', 'NONE');
#1723 = CARTESIAN_POINT ( 'NONE',  ( -0.5093500532425060401, -4.799145180956616130, 1.125000001365592306 ) ) ;
#1724 = CARTESIAN_POINT ( 'NONE',  ( 43.08845726811987475, -5.000000000000000000, 38.63139720814412925 ) ) ;
#1725 = VECTOR ( 'NONE', #10549, 1000.000000000000000 ) ;
#1726 = CYLINDRICAL_SURFACE ( 'NONE', #14159, 2.649999999999992806 ) ;
#1727 = DIRECTION ( 'NONE',  ( -0.000000000000000000, -1.000000000000000000, -0.000000000000000000 ) ) ;
#1728 = ORIENTED_EDGE ( 'NONE', *, *, #9373, .F. ) ;
#1729 = CARTESIAN_POINT ( 'NONE',  ( 3.061616997868383043E-15, -13.00000000000000178, 25.00000000000000000 ) ) ;
#1730 = CARTESIAN_POINT ( 'NONE',  ( 7.500000000000000000, 2.886751345948125547, -7.198902722707428481 ) ) ;
#1731 = DIRECTION ( 'NONE',  ( 1.000000000000000000, 0.000000000000000000, 0.000000000000000000 ) ) ;
#1732 = EDGE_CURVE ( 'NONE', #1275, #10154, #13943, .T. ) ;
#1733 = ORIENTED_EDGE ( 'NONE', *, *, #8308, .F. ) ;
#1734 = DIRECTION ( 'NONE',  ( -1.982541115402065110E-16, 1.000000000000000000, 0.000000000000000000 ) ) ;
#1735 = ORIENTED_EDGE ( 'NONE', *, *, #4357, .T. ) ;
#1736 = ORIENTED_EDGE ( 'NONE', *, *, #7501, .F. ) ;
#1737 = VECTOR ( 'NONE', #15330, 1000.000000000000000 ) ;
#1738 = CARTESIAN_POINT ( 'NONE',  ( 3.061616997868383141E-16, -24.75000000000000000, -5.000000000000000000 ) ) ;
#1739 = CARTESIAN_POINT ( 'NONE',  ( -2.712762565639006418, 3.052587955997511759, -3.430618716626627318 ) ) ;
#1740 = ADVANCED_BREP_SHAPE_REPRESENTATION ( '', ( #14760, #3223 ), #14881 ) ;
#1741 = CARTESIAN_POINT ( 'NONE',  ( 4.000000000000000000, -2.309401076758514915, -3.433295621305383349 ) ) ;
#1742 = AXIS2_PLACEMENT_3D ( 'NONE', #3072, #7933, #4514 ) ;
#1743 = CIRCLE ( 'NONE', #3807, 9.999999999999994671 ) ;
#1744 = CARTESIAN_POINT ( 'NONE',  ( 7.347880794884120722E-16, -13.00000000000000178, 6.000000000000000888 ) ) ;
#1745 = DIRECTION ( 'NONE',  ( 0.000000000000000000, 0.000000000000000000, -1.000000000000000000 ) ) ;
#1746 = DIRECTION ( 'NONE',  ( 0.4999999999999998335, 0.000000000000000000, 0.8660254037844387076 ) ) ;
#1747 = CIRCLE ( 'NONE', #3542, 1.999999999999998224 ) ;
#1748 = CARTESIAN_POINT ( 'NONE',  ( 57.73502691896258199, -4.999999999999997335, 2.081668171172168513E-14 ) ) ;
#1749 = LINE ( 'NONE', #12726, #1882 ) ;
#1750 = DIRECTION ( 'NONE',  ( 0.000000000000000000, 0.000000000000000000, 1.000000000000000000 ) ) ;
#1751 = CARTESIAN_POINT ( 'NONE',  ( 3.152801135295367541, -22.31250000136559564, -3.152801135295367541 ) ) ;
#1752 = CARTESIAN_POINT ( 'NONE',  ( 3.916244202832140253, -2.131511515620588160, -6.687499998634407028 ) ) ;
#1753 = ORIENTED_EDGE ( 'NONE', *, *, #4007, .F. ) ;
#1754 = AXIS2_PLACEMENT_3D ( 'NONE', #8234, #13131, #12807 ) ;
#1755 = DIRECTION ( 'NONE',  ( 0.000000000000000000, 1.000000000000000000, 0.000000000000000000 ) ) ;
#1756 = ADVANCED_FACE ( 'NONE', ( #11201, #8795 ), #13699, .T. ) ;
#1757 = ORIENTED_EDGE ( 'NONE', *, *, #102, .T. ) ;
#1758 = ORIENTED_EDGE ( 'NONE', *, *, #10314, .F. ) ;
#1759 = EDGE_CURVE ( 'NONE', #1476, #14724, #14936, .T. ) ;
#1760 = VECTOR ( 'NONE', #11899, 1000.000000000000000 ) ;
#1761 = PRODUCT_DEFINITION_SHAPE ( 'NONE', 'NONE',  #15974 ) ;
#1762 = CARTESIAN_POINT ( 'NONE',  ( -3.152801135295367096, -31.31250000136559564, -3.152801135295367541 ) ) ;
#1763 = CARTESIAN_POINT ( 'NONE',  ( -91.33974596215560382, -110.0591436588189396, -17.50000000000000000 ) ) ;
#1764 = VERTEX_POINT ( 'NONE', #2950 ) ;
#1765 = CONICAL_SURFACE ( 'NONE', #10292, 4.000000000000000000, 0.8911886515913786111 ) ;
#1766 = CARTESIAN_POINT ( 'NONE',  ( 5.000000000000003553, 1.275685995473128912E-14, -4.045263047592942307 ) ) ;
#1767 = CARTESIAN_POINT ( 'NONE',  ( 7.922798488042200660, -4.627419312545563379, -8.057411459260046982 ) ) ;
#1768 = CARTESIAN_POINT ( 'NONE',  ( 4.799145180956616130, -0.5093500532425063732, -6.374999998634408804 ) ) ;
#1769 = CARTESIAN_POINT ( 'NONE',  ( 2.982560088675708876, 3.325042182615861375, -0.3789984458506786558 ) ) ;
#1770 = CARTESIAN_POINT ( 'NONE',  ( 3.535533905932736864, -26.12500000000000355, 3.535533905932738641 ) ) ;
#1771 = CARTESIAN_POINT ( 'NONE',  ( 4.276409079477644148, 1.261996585732577891, -5.312499998634406140 ) ) ;
#1772 = CARTESIAN_POINT ( 'NONE',  ( 35.00000000000000000, 37.00000000000000000, -5.999999999999991118 ) ) ;
#1773 = FACE_OUTER_BOUND ( 'NONE', #13768, .T. ) ;
#1774 = CARTESIAN_POINT ( 'NONE',  ( 3.535533905932738197, -25.00000000273118417, -3.535533905932738197 ) ) ;
#1775 = DIRECTION ( 'NONE',  ( 0.000000000000000000, 0.000000000000000000, -1.000000000000000000 ) ) ;
#1776 = VECTOR ( 'NONE', #2352, 1000.000000000000227 ) ;
#1777 = CARTESIAN_POINT ( 'NONE',  ( -1.846868145590737420, -24.75000000136559564, 4.458734124999997661 ) ) ;
#1778 = ADVANCED_FACE ( 'NONE', ( #468, #3927 ), #8956, .F. ) ;
#1779 = CARTESIAN_POINT ( 'NONE',  ( 0.000000000000000000, 2.000000000000001776, -57.99999999999999289 ) ) ;
#1780 = ORIENTED_EDGE ( 'NONE', *, *, #11942, .T. ) ;
#1781 = ORIENTED_EDGE ( 'NONE', *, *, #734, .T. ) ;
#1782 = EDGE_CURVE ( 'NONE', #13190, #7075, #6857, .T. ) ;
#1783 = CARTESIAN_POINT ( 'NONE',  ( -7.500000000000001776, 4.651022038490038923, -7.928862870699877163 ) ) ;
#1784 = EDGE_LOOP ( 'NONE', ( #12318, #3642, #1, #11085, #9014 ) ) ;
#1785 = LINE ( 'NONE', #3156, #7127 ) ;
#1786 = VECTOR ( 'NONE', #14776, 1000.000000000000000 ) ;
#1787 = VERTEX_POINT ( 'NONE', #386 ) ;
#1788 = CARTESIAN_POINT ( 'NONE',  ( 0.000000000000000000, -20.00000000000000000, 0.000000000000000000 ) ) ;
#1789 = FACE_OUTER_BOUND ( 'NONE', #851, .T. ) ;
#1790 = CARTESIAN_POINT ( 'NONE',  ( -1.846868145590734756, -26.37500000136559564, -4.458734125000000326 ) ) ;
#1791 = CARTESIAN_POINT ( 'NONE',  ( -4.999999999999848121, 1.272547481429012750, -0.4615974799134661688 ) ) ;
#1792 = PRODUCT_CONTEXT ( 'NONE', #13090, 'mechanical' ) ;
#1793 = CARTESIAN_POINT ( 'NONE',  ( -2.131511515620587272, -3.916244202832140253, -7.937499998634408804 ) ) ;
#1794 = CARTESIAN_POINT ( 'NONE',  ( 1.261996585732578113, -4.276409079477644148, 0.1875000013655918341 ) ) ;
#1795 = ORIENTED_EDGE ( 'NONE', *, *, #819, .T. ) ;
#1796 = EDGE_CURVE ( 'NONE', #15821, #6007, #5306, .T. ) ;
#1797 = SHAPE_REPRESENTATION_RELATIONSHIP ( 'NONE' , 'NONE' ,  #7495, #10261 ) ;
#1798 = ORIENTED_EDGE ( 'NONE', *, *, #688, .F. ) ;
#1799 = CARTESIAN_POINT ( 'NONE',  ( 2.500000000000000000, 2.357898499370433054, -1.951563910473907981E-15 ) ) ;
#1800 = ORIENTED_EDGE ( 'NONE', *, *, #9107, .F. ) ;
#1801 = CARTESIAN_POINT ( 'NONE',  ( 4.209348295687701302, 3.401574460001766109, -4.937500000000000888 ) ) ;
#1802 = DIRECTION ( 'NONE',  ( -0.000000000000000000, -1.000000000000000000, -0.000000000000000000 ) ) ;
#1803 = DIRECTION ( 'NONE',  ( -0.000000000000000000, -1.000000000000000000, -0.000000000000000000 ) ) ;
#1804 = CARTESIAN_POINT ( 'NONE',  ( 4.799145180956616130, -0.5093500532425063732, 1.375000001365592528 ) ) ;
#1805 = DIRECTION ( 'NONE',  ( 0.5000000000000001110, 7.511572993685796142E-16, -0.8660254037844387076 ) ) ;
#1806 = DIRECTION ( 'NONE',  ( 0.000000000000000000, 0.000000000000000000, 1.000000000000000000 ) ) ;
#1807 = LINE ( 'NONE', #10626, #4265 ) ;
#1808 = EDGE_LOOP ( 'NONE', ( #14146, #8988, #5187, #10193, #12157, #10854 ) ) ;
#1809 = DIRECTION ( 'NONE',  ( -3.343241100358131282E-16, 0.000000000000000000, 1.000000000000000000 ) ) ;
#1810 = DIRECTION ( 'NONE',  ( 3.343241100358131282E-16, -0.000000000000000000, -1.000000000000000000 ) ) ;
#1811 = EDGE_CURVE ( 'NONE', #1275, #3694, #5749, .T. ) ;
#1812 = CARTESIAN_POINT ( 'NONE',  ( 5.040301471719072168, 5.750234626350511746, -0.09933465333850965973 ) ) ;
#1813 = ORIENTED_EDGE ( 'NONE', *, *, #12598, .F. ) ;
#1814 = CARTESIAN_POINT ( 'NONE',  ( 4.420982230657666712, -0.5789871446316176007, -0.3789984458506777676 ) ) ;
#1815 = ORIENTED_EDGE ( 'NONE', *, *, #11551, .T. ) ;
#1816 = VERTEX_POINT ( 'NONE', #7825 ) ;
#1817 = DIRECTION ( 'NONE',  ( 0.000000000000000000, 0.000000000000000000, 1.000000000000000000 ) ) ;
#1818 = DIRECTION ( 'NONE',  ( 0.000000000000000000, 0.000000000000000000, -1.000000000000000000 ) ) ;
#1819 = CARTESIAN_POINT ( 'NONE',  ( -7.500000000000005329, 0.3744244963005067262, -3.022637072276969577E-15 ) ) ;
#1820 = EDGE_CURVE ( 'NONE', #8371, #10126, #2129, .T. ) ;
#1821 = CARTESIAN_POINT ( 'NONE',  ( 3.535533905932736864, -26.25000000273118417, 3.535533905932738641 ) ) ;
#1822 = CYLINDRICAL_SURFACE ( 'NONE', #11417, 39.99999999999999289 ) ;
#1823 = LINE ( 'NONE', #8147, #2279 ) ;
#1824 = CARTESIAN_POINT ( 'NONE',  ( -3.401574460001764777, 4.209348295687701302, -7.687500000000004441 ) ) ;
#1825 = CARTESIAN_POINT ( 'NONE',  ( 6.123233995736766282E-16, -20.00000000000000000, -5.000000000000000000 ) ) ;
#1826 = DIRECTION ( 'NONE',  ( 0.000000000000000000, 1.000000000000000000, 0.000000000000000000 ) ) ;
#1827 = CARTESIAN_POINT ( 'NONE',  ( 3.152801135295366208, -23.56250000136559564, 3.152801135295367985 ) ) ;
#1828 = CARTESIAN_POINT ( 'NONE',  ( -2.131511515620587272, -3.916244202832140253, -4.937499998634406140 ) ) ;
#1829 = ORIENTED_EDGE ( 'NONE', *, *, #7686, .F. ) ;
#1830 = CARTESIAN_POINT ( 'NONE',  ( 6.250000000000000888, 5.051814855409223703, -7.198902722707425816 ) ) ;
#1831 = ORIENTED_EDGE ( 'NONE', *, *, #11856, .T. ) ;
#1832 = EDGE_LOOP ( 'NONE', ( #10362, #15744, #11743, #14616, #184, #15244, #1199, #12170 ) ) ;
#1833 = CARTESIAN_POINT ( 'NONE',  ( 3.152801135295366208, -21.56250000136559208, 3.152801135295367985 ) ) ;
#1834 = CARTESIAN_POINT ( 'NONE',  ( 0.000000000000000000, 1.178949249685213863, -2.042000000000001148 ) ) ;
#1835 = ORIENTED_EDGE ( 'NONE', *, *, #1935, .T. ) ;
#1836 = DIRECTION ( 'NONE',  ( -1.000000000000000000, -0.000000000000000000, -0.000000000000000000 ) ) ;
#1837 = B_SPLINE_CURVE_WITH_KNOTS ( 'NONE', 3,
 ( #5625, #11908, #11598, #4165, #9422, #15333 ),
 .UNSPECIFIED., .F., .F.,
 ( 4, 2, 4 ),
 ( 2.475503369179729800E-07, 0.002222330217055626302, 0.004444412883774334112 ),
 .UNSPECIFIED. ) ;
#1838 = DIRECTION ( 'NONE',  ( 0.000000000000000000, 0.000000000000000000, -1.000000000000000000 ) ) ;
#1839 = ADVANCED_FACE ( 'NONE', ( #1661 ), #3169, .F. ) ;
#1840 = CARTESIAN_POINT ( 'NONE',  ( -0.5093500532425060401, -4.799145180956616130, -3.624999998634407916 ) ) ;
#1841 = FACE_OUTER_BOUND ( 'NONE', #15839, .T. ) ;
#1842 = ADVANCED_FACE ( 'NONE', ( #6693 ), #12887, .F. ) ;
#1843 = CARTESIAN_POINT ( 'NONE',  ( -2.071067811865475061, -24.68750000000000355, -5.000000000000000888 ) ) ;
#1844 = CARTESIAN_POINT ( 'NONE',  ( 1.261996585732578113, -4.276409079477644148, -7.562499998634407916 ) ) ;
#1845 = DIRECTION ( 'NONE',  ( -0.000000000000000000, 1.000000000000000000, -0.000000000000000000 ) ) ;
#1846 = CARTESIAN_POINT ( 'NONE',  ( -21.01110699893060030, 2.000000000000000000, 36.39230484541324273 ) ) ;
#1847 = CARTESIAN_POINT ( 'NONE',  ( -2.071067811865475061, -23.81250000273118772, -5.000000000000000888 ) ) ;
#1848 = VERTEX_POINT ( 'NONE', #12962 ) ;
#1849 = CARTESIAN_POINT ( 'NONE',  ( 4.458734124999997661, -25.50000000136559919, 1.846868145590737864 ) ) ;
#1850 = CARTESIAN_POINT ( 'NONE',  ( 4.209348295687701302, 3.401574460001766109, -6.937500000000003553 ) ) ;
#1851 = EDGE_LOOP ( 'NONE', ( #10259, #13734, #246, #14447 ) ) ;
#1852 = ORIENTED_EDGE ( 'NONE', *, *, #10275, .F. ) ;
#1853 = CARTESIAN_POINT ( 'NONE',  ( -35.00000000000000000, 37.00000000000000000, 2.649999999999985700 ) ) ;
#1854 = DIRECTION ( 'NONE',  ( 9.048317650695024227E-15, 0.000000000000000000, 1.000000000000000000 ) ) ;
#1855 = AXIS2_PLACEMENT_3D ( 'NONE', #12682, #10206, #10293 ) ;
#1856 = ORIENTED_EDGE ( 'NONE', *, *, #8793, .T. ) ;
#1857 = FACE_OUTER_BOUND ( 'NONE', #10826, .T. ) ;
#1858 = CARTESIAN_POINT ( 'NONE',  ( -89.99999999999997158, -95.00000000000001421, 13.35786437626905965 ) ) ;
#1859 = ADVANCED_FACE ( 'NONE', ( #14115 ), #10400, .T. ) ;
#1860 = CARTESIAN_POINT ( 'NONE',  ( 1.846868145590736310, -25.87500000136559919, 4.458734124999999437 ) ) ;
#1861 = FACE_OUTER_BOUND ( 'NONE', #5695, .T. ) ;
#1862 = CARTESIAN_POINT ( 'NONE',  ( 42.02221399786069611, -3.000000000000001332, 2.650000000000089617 ) ) ;
#1863 = SHAPE_DEFINITION_REPRESENTATION ( #4609, #14733 ) ;
#1864 = CARTESIAN_POINT ( 'NONE',  ( 4.209348295687701302, 3.401574460001766109, -7.812499997268815832 ) ) ;
#1865 = CARTESIAN_POINT ( 'NONE',  ( -5.000000000000003553, -1.404940523648820476E-14, -7.420263044861759028 ) ) ;
#1866 = AXIS2_PLACEMENT_3D ( 'NONE', #14603, #3524, #3687 ) ;
#1867 = ORIENTED_EDGE ( 'NONE', *, *, #12222, .T. ) ;
#1868 =( NAMED_UNIT ( * ) SI_UNIT ( $, .STERADIAN. ) SOLID_ANGLE_UNIT ( ) );
#1869 = ORIENTED_EDGE ( 'NONE', *, *, #7311, .F. ) ;
#1870 = FACE_OUTER_BOUND ( 'NONE', #15786, .T. ) ;
#1871 = ORIENTED_EDGE ( 'NONE', *, *, #4747, .T. ) ;
#1872 = ITEM_DEFINED_TRANSFORMATION ( 'NONE', 'NONE', #11215,  #3223 ) ;
#1873 = CIRCLE ( 'NONE', #7573, 2.100000000000000089 ) ;
#1874 = CARTESIAN_POINT ( 'NONE',  ( -1.415196051561583790, 4.795541693661363958, -4.750000000000000888 ) ) ;
#1875 = EDGE_CURVE ( 'NONE', #11646, #2119, #5705, .T. ) ;
#1876 = CIRCLE ( 'NONE', #3686, 2.649999999999985700 ) ;
#1877 = EDGE_CURVE ( 'NONE', #12259, #8828, #854, .T. ) ;
#1878 = ADVANCED_FACE ( 'NONE', ( #8145 ), #4490, .T. ) ;
#1879 = DIRECTION ( 'NONE',  ( 0.000000000000000000, 0.000000000000000000, 1.000000000000000000 ) ) ;
#1880 = CARTESIAN_POINT ( 'NONE',  ( -39.99999999999999289, -9.000000000000001776, -2.500000000000079492 ) ) ;
#1882 = VECTOR ( 'NONE', #1665, 1000.000000000000000 ) ;
#1881 = CARTESIAN_POINT ( 'NONE',  ( 0.5093500532425063732, 4.799145180956616130, 0.6250000013655918618 ) ) ;
#1883 = CARTESIAN_POINT ( 'NONE',  ( 4.795541693661363958, 1.415196051561583790, -1.000000000000000888 ) ) ;
#1884 = CYLINDRICAL_SURFACE ( 'NONE', #12589, 2.000000000000000888 ) ;
#1885 = DIRECTION ( 'NONE',  ( 0.000000000000000000, 0.000000000000000000, 1.000000000000000000 ) ) ;
#1886 = VERTEX_POINT ( 'NONE', #9424 ) ;
#1887 = CARTESIAN_POINT ( 'NONE',  ( 7.500000000000000888, 0.3744244963005068927, 1.477225460011500186E-15 ) ) ;
#1888 = FACE_BOUND ( 'NONE', #13265, .T. ) ;
#1889 = EDGE_LOOP ( 'NONE', ( #3943, #12784, #12058, #10841 ) ) ;
#1890 = PLANE ( 'NONE',  #14444 ) ;
#1891 = ORIENTED_EDGE ( 'NONE', *, *, #625, .T. ) ;
#1892 = ORIENTED_EDGE ( 'NONE', *, *, #8122, .T. ) ;
#1893 = DIRECTION ( 'NONE',  ( -0.000000000000000000, -1.000000000000000000, -0.000000000000000000 ) ) ;
#1894 = DIRECTION ( 'NONE',  ( 1.000000000000000000, 0.000000000000000000, 0.000000000000000000 ) ) ;
#1895 = ADVANCED_FACE ( 'NONE', ( #9348 ), #1822, .T. ) ;
#1896 = CARTESIAN_POINT ( 'NONE',  ( 35.00000000000000000, 40.00000000000000000, 0.000000000000000000 ) ) ;
#1897 = ADVANCED_FACE ( 'NONE', ( #3041 ), #4340, .T. ) ;
#1898 = CARTESIAN_POINT ( 'NONE',  ( -4.000000000000000000, -2.309401076758515803, -0.4999999999999995559 ) ) ;
#1899 = DIRECTION ( 'NONE',  ( -0.8660254037844373753, 0.5000000000000021094, 0.000000000000000000 ) ) ;
#1900 = CARTESIAN_POINT ( 'NONE',  ( 4.000000000000000000, -2.309401076758516691, -0.4999999999999995559 ) ) ;
#1901 = CARTESIAN_POINT ( 'NONE',  ( 6.901579824520445605, -4.675625068323825850, -0.7022220667781389203 ) ) ;
#1902 = PLANE ( 'NONE',  #13101 ) ;
#1903 = FACE_OUTER_BOUND ( 'NONE', #4290, .T. ) ;
#1904 = CARTESIAN_POINT ( 'NONE',  ( 4.458734124999999437, -28.68750000136559564, 0.000000000000000000 ) ) ;
#1905 =( BOUNDED_CURVE ( )  B_SPLINE_CURVE ( 3, ( #6211, #13529, #3857, #9909 ),
 .UNSPECIFIED., .F., .F. ) 
 B_SPLINE_CURVE_WITH_KNOTS ( ( 4, 4 ),
 ( 1.570796326794895226, 3.141592653589793116 ),
 .UNSPECIFIED. ) 
 CURVE ( )  GEOMETRIC_REPRESENTATION_ITEM ( )  RATIONAL_B_SPLINE_CURVE ( ( 1.000000000000000000, 0.8047378541243646044, 0.8047378541243646044, 1.000000000000000000 ) ) 
 REPRESENTATION_ITEM ( '' )  );
#1906 = SHAPE_REPRESENTATION ( 'pin2', ( #3223 ), #5534 ) ;
#1907 = CARTESIAN_POINT ( 'NONE',  ( -3.753672977998669946, -3.033343224707661712, -0.7499999986344074721 ) ) ;
#1908 = EDGE_LOOP ( 'NONE', ( #2842, #14498, #3720, #9541 ) ) ;
#1909 = CARTESIAN_POINT ( 'NONE',  ( 0.000000000000000000, 1.178949249685213863, -2.042000000000001148 ) ) ;
#1910 = EDGE_LOOP ( 'NONE', ( #3150, #8237 ) ) ;
#1911 = ORIENTED_EDGE ( 'NONE', *, *, #7555, .T. ) ;
#1912 = SURFACE_SIDE_STYLE ('',( #4264 ) ) ;
#1913 = CARTESIAN_POINT ( 'NONE',  ( -4.458734125000001214, -25.12500000136559564, 1.846868145590734089 ) ) ;
#1914 = LINE ( 'NONE', #2077, #1445 ) ;
#1915 = DIRECTION ( 'NONE',  ( 0.000000000000000000, 0.000000000000000000, -1.000000000000000000 ) ) ;
#1916 = AXIS2_PLACEMENT_3D ( 'NONE', #14309, #3234, #12422 ) ;
#1917 = CARTESIAN_POINT ( 'NONE',  ( 5.000000000000002665, 0.000000000000000000, -2.700000000000001066 ) ) ;
#1918 = CARTESIAN_POINT ( 'NONE',  ( -4.276409079477644148, -1.261996585732578335, -3.812499998634404808 ) ) ;
#1919 = DIRECTION ( 'NONE',  ( 0.4999999999999997224, 0.000000000000000000, 0.8660254037844388186 ) ) ;
#1920 = CARTESIAN_POINT ( 'NONE',  ( 3.061616997868383141E-16, -25.75000000000000355, -5.000000000000000000 ) ) ;
#1921 = CARTESIAN_POINT ( 'NONE',  ( 4.391654775818395251, -2.390265326283149694, 1.874999999999998224 ) ) ;
#1922 = DIRECTION ( 'NONE',  ( 1.000000000000000000, 0.000000000000000000, 0.000000000000000000 ) ) ;
#1923 = FACE_OUTER_BOUND ( 'NONE', #1908, .T. ) ;
#1924 = CARTESIAN_POINT ( 'NONE',  ( 3.152801135295367541, -29.31250000136559208, -3.152801135295367541 ) ) ;
#1925 = VERTEX_POINT ( 'NONE', #10482 ) ;
#1926 = AXIS2_PLACEMENT_3D ( 'NONE', #3573, #10850, #11966 ) ;
#1927 = CARTESIAN_POINT ( 'NONE',  ( 4.458734124999999437, -27.43750000136559564, 0.000000000000000000 ) ) ;
#1928 = CARTESIAN_POINT ( 'NONE',  ( 5.088535779736900189, -5.722386535632459470, -7.491772860716841897 ) ) ;
#1929 = VERTEX_POINT ( 'NONE', #1983 ) ;
#1930 = EDGE_LOOP ( 'NONE', ( #5183, #3848, #7111, #15399 ) ) ;
#1932 = CARTESIAN_POINT ( 'NONE',  ( 0.3461262719736147297, -4.658553426539303821, -3.671615880910379381 ) ) ;
#1931 = VECTOR ( 'NONE', #6950, 1000.000000000000000 ) ;
#1933 = ADVANCED_FACE ( 'NONE', ( #14354, #11835, #11910, #783, #3283, #4415 ), #5777, .T. ) ;
#1934 = CARTESIAN_POINT ( 'NONE',  ( 4.999999999999845457, -1.272547481429021854, -6.961597479913466557 ) ) ;
#1935 = EDGE_CURVE ( 'NONE', #15134, #2381, #9873, .T. ) ;
#1936 = ORIENTED_EDGE ( 'NONE', *, *, #15075, .F. ) ;
#1937 = CARTESIAN_POINT ( 'NONE',  ( -5.000000000000000888, -24.68750000273118772, -2.071067811865475949 ) ) ;
#1938 =( GEOMETRIC_REPRESENTATION_CONTEXT ( 3 ) GLOBAL_UNCERTAINTY_ASSIGNED_CONTEXT ( ( #7400 ) ) GLOBAL_UNIT_ASSIGNED_CONTEXT ( ( #14406, #828, #1868 ) ) REPRESENTATION_CONTEXT ( 'NONE', 'WORKASPACE' ) );
#1939 = VECTOR ( 'NONE', #2696, 1000.000000000000227 ) ;
#1940 = CARTESIAN_POINT ( 'NONE',  ( -24.26932219902320043, 20.00000000000000000, 5.999999999999998224 ) ) ;
#1941 = VECTOR ( 'NONE', #5042, 1000.000000000000114 ) ;
#1942 = CARTESIAN_POINT ( 'NONE',  ( 4.458734125000000326, -25.62500000136559564, -1.846868145590734978 ) ) ;
#1943 = CARTESIAN_POINT ( 'NONE',  ( 5.000000000000003553, 1.275685995473128912E-14, -5.045263047592944083 ) ) ;
#1944 = CARTESIAN_POINT ( 'NONE',  ( 3.401574460001763445, -4.209348295687703079, -0.06249999726881656087 ) ) ;
#1945 = APPLICATION_PROTOCOL_DEFINITION ( 'draft international standard', 'automotive_design', 1998, #13090 ) ;
#1946 = CARTESIAN_POINT ( 'NONE',  ( 2.500000000000000444, -7.216878364870333407, -7.063244554130006847 ) ) ;
#1947 = CARTESIAN_POINT ( 'NONE',  ( -5.000000000000000888, 6.123233995736767268E-16, -25.03750572909317285 ) ) ;
#1948 = ORIENTED_EDGE ( 'NONE', *, *, #5298, .T. ) ;
#1949 = VECTOR ( 'NONE', #2580, 1000.000000000000000 ) ;
#1951 = EDGE_LOOP ( 'NONE', ( #3605, #5125, #8000, #7015, #1453, #6014, #15457, #9265, #5583, #6594, #755, #6379 ) ) ;
#1950 = EDGE_CURVE ( 'NONE', #11709, #1967, #4570, .T. ) ;
#1952 = CARTESIAN_POINT ( 'NONE',  ( -7.112481253774269874, 4.553861071372323543, -7.781689322728262859 ) ) ;
#1953 = EDGE_CURVE ( 'NONE', #13669, #12414, #6650, .T. ) ;
#1954 = CIRCLE ( 'NONE', #9691, 40.00000000000000711 ) ;
#1955 = VERTEX_POINT ( 'NONE', #7246 ) ;
#1956 = AXIS2_PLACEMENT_3D ( 'NONE', #5648, #14133, #3063 ) ;
#1957 = APPLICATION_CONTEXT ( 'automotive_design' ) ;
#1958 = CARTESIAN_POINT ( 'NONE',  ( 35.00000000000000000, 40.00000000000000000, 2.649999999999983924 ) ) ;
#1959 = CARTESIAN_POINT ( 'NONE',  ( -115.0000000000000142, -10.00000000000000888, 7.500000000000001776 ) ) ;
#1960 = CARTESIAN_POINT ( 'NONE',  ( 3.401574460001763445, -4.209348295687703079, -8.062499997268812280 ) ) ;
#1961 = VECTOR ( 'NONE', #15902, 1000.000000000000000 ) ;
#1962 = CARTESIAN_POINT ( 'NONE',  ( -4.391654775818395251, 2.390265326283148806, -6.499999997268815832 ) ) ;
#1963 = CIRCLE ( 'NONE', #12544, 4.000000000000000000 ) ;
#1964 = SURFACE_SIDE_STYLE ('',( #13024 ) ) ;
#1965 = CARTESIAN_POINT ( 'NONE',  ( 4.729367062499999719, -21.84375000068279604, 0.000000000000000000 ) ) ;
#1966 = CARTESIAN_POINT ( 'NONE',  ( 16.55500000000001393, 0.000000000000000000, 0.000000000000000000 ) ) ;
#1967 = VERTEX_POINT ( 'NONE', #4808 ) ;
#1968 = CARTESIAN_POINT ( 'NONE',  ( 6.000000000000000000, -13.00000000000000178, -1.500000000000000000 ) ) ;
#1969 = LINE ( 'NONE', #11661, #8441 ) ;
#1970 = DIRECTION ( 'NONE',  ( 0.000000000000000000, 0.000000000000000000, -1.000000000000000000 ) ) ;
#1971 = EDGE_CURVE ( 'NONE', #2273, #15878, #13430, .T. ) ;
#1972 = ORIENTED_EDGE ( 'NONE', *, *, #10703, .T. ) ;
#1973 = CARTESIAN_POINT ( 'NONE',  ( -9.184850993605147944E-16, -27.25000000000000000, 5.000000000000000000 ) ) ;
#1974 = ORIENTED_EDGE ( 'NONE', *, *, #5141, .T. ) ;
#1975 = EDGE_CURVE ( 'NONE', #6779, #6035, #6277, .T. ) ;
#1976 = ORIENTED_EDGE ( 'NONE', *, *, #8220, .F. ) ;
#1977 = CARTESIAN_POINT ( 'NONE',  ( 2.131511515620586383, 3.916244202832140253, -0.4374999986344086933 ) ) ;
#1978 = CYLINDRICAL_SURFACE ( 'NONE', #13067, 5.000000000000000000 ) ;
#1979 = AXIS2_PLACEMENT_3D ( 'NONE', #2128, #11091, #15945 ) ;
#1980 = CARTESIAN_POINT ( 'NONE',  ( -7.500000000000004441, 2.575910028905296301, -0.3641256808890121488 ) ) ;
#1981 = FACE_OUTER_BOUND ( 'NONE', #7072, .T. ) ;
#1983 = CARTESIAN_POINT ( 'NONE',  ( 5.000000000000004441, 0.000000000000000000, 4.250000000000000000 ) ) ;
#1982 = VECTOR ( 'NONE', #15334, 1000.000000000000000 ) ;
#1984 = CARTESIAN_POINT ( 'NONE',  ( 5.000000000000000888, -22.93749999999999645, -2.071067811865475505 ) ) ;
#1985 = CARTESIAN_POINT ( 'NONE',  ( -41.99999999999978684, -9.000000000000001776, 3.499999999999998668 ) ) ;
#1986 = FACE_OUTER_BOUND ( 'NONE', #5078, .T. ) ;
#1987 = CARTESIAN_POINT ( 'NONE',  ( 2.500000000000000000, 0.000000000000000000, 0.000000000000000000 ) ) ;
#1988 = CARTESIAN_POINT ( 'NONE',  ( -8.190561711645485556E-16, -27.93750000136559564, 4.458734124999999437 ) ) ;
#1989 = PRODUCT_DEFINITION_FORMATION_WITH_SPECIFIED_SOURCE ( 'ANY', '', #3575, .NOT_KNOWN. ) ;
#1990 = CARTESIAN_POINT ( 'NONE',  ( -0.5093500532425060401, -4.799145180956616130, 1.375000001365592528 ) ) ;
#1991 = ORIENTED_EDGE ( 'NONE', *, *, #9830, .F. ) ;
#1992 = DIRECTION ( 'NONE',  ( -0.000000000000000000, -1.000000000000000000, -0.000000000000000000 ) ) ;
#1993 = ORIENTED_EDGE ( 'NONE', *, *, #6721, .F. ) ;
#1994 = VERTEX_POINT ( 'NONE', #11032 ) ;
#1995 = EDGE_CURVE ( 'NONE', #14464, #5100, #13505, .T. ) ;
#1996 = SURFACE_STYLE_USAGE ( .BOTH. , #11997 ) ;
#1997 = CARTESIAN_POINT ( 'NONE',  ( 1.846868145590735200, -27.50000000136559208, -4.458734125000000326 ) ) ;
#1998 = CARTESIAN_POINT ( 'NONE',  ( 4.795541693661363958, 1.415196051561583790, -8.000000000000003553 ) ) ;
#1999 = AXIS2_PLACEMENT_3D ( 'NONE', #10864, #15807, #4723 ) ;
#2000 = DIRECTION ( 'NONE',  ( -0.000000000000000000, 1.000000000000000000, -0.000000000000000000 ) ) ;
#2001 = AXIS2_PLACEMENT_3D ( 'NONE', #431, #4458, #1629 ) ;
#2002 = CYLINDRICAL_SURFACE ( 'NONE', #6173, 5.000000000000000888 ) ;
#2003 = CARTESIAN_POINT ( 'NONE',  ( -2.131511515620587272, -3.916244202832140253, -4.687499998634405252 ) ) ;
#2004 = CARTESIAN_POINT ( 'NONE',  ( 3.750000000000005773, 6.495190528383288253, 0.000000000000000000 ) ) ;
#2005 =( BOUNDED_CURVE ( )  B_SPLINE_CURVE ( 2, ( #11690, #4431, #643, #12979, #5568, #15436, #3212, #15588, #11614, #565, #9294 ),
 .UNSPECIFIED., .F., .F. ) 
 B_SPLINE_CURVE_WITH_KNOTS ( ( 3, 2, 2, 2, 2, 3 ),
 ( 0.8045872658012773737, 0.8125000000000000000, 0.8249999999999999556, 0.8375000000000000222, 0.8499999999999999778, 0.8545872658012773071 ),
 .UNSPECIFIED. ) 
 CURVE ( )  GEOMETRIC_REPRESENTATION_ITEM ( )  RATIONAL_B_SPLINE_CURVE ( ( 0.9646335149384803742, 0.9518143178943441196, 1.000000000000000000, 0.9238795325112867385, 1.000000000000000000, 0.9238795325112867385, 1.000000000000000000, 0.9238795325112867385, 1.000000000000000000, 0.9720652146169428409, 0.9646335149384808183 ) ) 
 REPRESENTATION_ITEM ( '' )  );
#2006 = CARTESIAN_POINT ( 'NONE',  ( 5.000000000000000000, -24.06250000000000000, 2.071067811865478614 ) ) ;
#2007 = CARTESIAN_POINT ( 'NONE',  ( -0.5711823568785978633, -5.381735091635035495, 1.687499999999998446 ) ) ;
#2008 = CARTESIAN_POINT ( 'NONE',  ( -21.01110699893060030, -3.000000000000000000, 36.39230484541324273 ) ) ;
#2009 = VECTOR ( 'NONE', #13532, 1000.000000000000114 ) ;
#2010 = DIRECTION ( 'NONE',  ( 0.000000000000000000, 0.000000000000000000, 1.000000000000000000 ) ) ;
#2011 = CARTESIAN_POINT ( 'NONE',  ( -5.000000000000000888, -21.56250000273118772, 2.071067811865474617 ) ) ;
#2012 = ORIENTED_EDGE ( 'NONE', *, *, #4980, .F. ) ;
#2013 = CARTESIAN_POINT ( 'NONE',  ( 4.458734124999997661, -23.50000000136559564, 1.846868145590737864 ) ) ;
#2014 = FACE_OUTER_BOUND ( 'NONE', #2418, .T. ) ;
#2015 = ORIENTED_EDGE ( 'NONE', *, *, #11671, .T. ) ;
#2016 = ORIENTED_EDGE ( 'NONE', *, *, #6491, .F. ) ;
#2017 = CARTESIAN_POINT ( 'NONE',  ( 2.500000000000000000, -1.178949249685213863, 2.042000000000002924 ) ) ;
#2018 = EDGE_CURVE ( 'NONE', #12914, #3405, #5417, .T. ) ;
#2019 = VECTOR ( 'NONE', #7235, 1000.000000000000000 ) ;
#2020 = CARTESIAN_POINT ( 'NONE',  ( 4.458734125000000326, -30.37500000136559564, -1.846868145590734978 ) ) ;
#2021 = CARTESIAN_POINT ( 'NONE',  ( -4.000000000000000000, 2.309401076758498483, -0.4999999999999927280 ) ) ;
#2022 = ORIENTED_EDGE ( 'NONE', *, *, #3556, .F. ) ;
#2023 = CARTESIAN_POINT ( 'NONE',  ( -45.00000000000000000, 0.000000000000000000, 17.50000000000000000 ) ) ;
#2024 = COLOUR_RGB ( '', 0.72549020, 0.75294118, 0.79215686) ;
#2025 = AXIS2_PLACEMENT_3D ( 'NONE', #2781, #6510, #13683 ) ;
#2026 = CARTESIAN_POINT ( 'NONE',  ( 3.061616997868383141E-16, -23.75000000000000000, -5.000000000000000000 ) ) ;
#2027 = CARTESIAN_POINT ( 'NONE',  ( 3.152801135295366208, -26.81250000136559564, 3.152801135295367985 ) ) ;
#2028 = VECTOR ( 'NONE', #3808, 1000.000000000000114 ) ;
#2029 = CARTESIAN_POINT ( 'NONE',  ( 0.000000000000000000, 20.00000000000000000, 0.000000000000000000 ) ) ;
#2030 = ADVANCED_FACE ( 'NONE', ( #12219 ), #3594, .T. ) ;
#2031 = CARTESIAN_POINT ( 'NONE',  ( 5.000000000000000000, -31.00000000000000000, 0.000000000000000000 ) ) ;
#2032 = CARTESIAN_POINT ( 'NONE',  ( 4.204015924366189871, -1.626724848190933548, -3.610627190413393084 ) ) ;
#2033 = VECTOR ( 'NONE', #10246, 1000.000000000000000 ) ;
#2034 = ORIENTED_EDGE ( 'NONE', *, *, #8902, .F. ) ;
#2035 = CIRCLE ( 'NONE', #4097, 2.649999999999985700 ) ;
#2036 = VERTEX_POINT ( 'NONE', #3668 ) ;
#2037 = DIRECTION ( 'NONE',  ( 0.000000000000000000, -1.000000000000000000, 0.000000000000000000 ) ) ;
#2038 = ORIENTED_EDGE ( 'NONE', *, *, #13694, .F. ) ;
#2039 = DIRECTION ( 'NONE',  ( 0.000000000000000000, 0.000000000000000000, 1.000000000000000000 ) ) ;
#2040 = DIRECTION ( 'NONE',  ( 0.000000000000000000, 0.000000000000000000, -1.000000000000000000 ) ) ;
#2041 = AXIS2_PLACEMENT_3D ( 'NONE', #9494, #3190, #14264 ) ;
#2042 = EDGE_CURVE ( 'NONE', #15020, #15896, #12067, .T. ) ;
#2043 = CARTESIAN_POINT ( 'NONE',  ( 3.753672977998667726, 3.033343224707664376, 0.7500000013655939712 ) ) ;
#2044 = EDGE_CURVE ( 'NONE', #7914, #615, #1590, .T. ) ;
#2045 = DIRECTION ( 'NONE',  ( -0.000000000000000000, -1.000000000000000000, -0.000000000000000000 ) ) ;
#2046 = CARTESIAN_POINT ( 'NONE',  ( 4.795541693661363958, 1.415196051561583790, -8.874999997268814056 ) ) ;
#2047 = DIRECTION ( 'NONE',  ( -0.5000000000000002220, 1.734723475976806503E-15, -0.8660254037844383745 ) ) ;
#2048 = CARTESIAN_POINT ( 'NONE',  ( 1.411581201560190495E-15, 4.862606272033091592, -3.745885042887436622 ) ) ;
#2049 = DIRECTION ( 'NONE',  ( -1.000000000000000000, -0.000000000000000000, -0.000000000000000000 ) ) ;
#2050 = ORIENTED_EDGE ( 'NONE', *, *, #6025, .T. ) ;
#2051 = DIRECTION ( 'NONE',  ( -1.000000000000000000, 0.000000000000000000, 0.000000000000000000 ) ) ;
#2052 = CARTESIAN_POINT ( 'NONE',  ( -6.259644161404860030E-16, -4.618802153517027165, -3.433295621305388234 ) ) ;
#2053 = LINE ( 'NONE', #10784, #5284 ) ;
#2054 = ORIENTED_EDGE ( 'NONE', *, *, #4567, .T. ) ;
#2055 = CARTESIAN_POINT ( 'NONE',  ( -114.4056415360013688, -110.1959696241292335, 7.500000000000001776 ) ) ;
#2056 = VERTEX_POINT ( 'NONE', #6022 ) ;
#2057 = ORIENTED_EDGE ( 'NONE', *, *, #7517, .T. ) ;
#2058 = DIRECTION ( 'NONE',  ( 0.000000000000000000, 0.000000000000000000, -1.000000000000000000 ) ) ;
#2059 = DIRECTION ( 'NONE',  ( 0.000000000000000000, 0.000000000000000000, 1.000000000000000000 ) ) ;
#2060 = CARTESIAN_POINT ( 'NONE',  ( -116.3391301858327296, -120.2076149402627294, -7.500000000000000000 ) ) ;
#2061 = EDGE_CURVE ( 'NONE', #14193, #7180, #15739, .T. ) ;
#2062 = CARTESIAN_POINT ( 'NONE',  ( 4.999999999999848121, -1.272547481429015859, -5.086597482644648061 ) ) ;
#2063 = CARTESIAN_POINT ( 'NONE',  ( -28.86751345948129455, -4.999999999999997335, 49.99999999999999289 ) ) ;
#2064 = ADVANCED_FACE ( 'NONE', ( #11108 ), #13198, .T. ) ;
#2065 = CARTESIAN_POINT ( 'NONE',  ( -5.000000000000000888, -29.56250000273118417, 2.071067811865474617 ) ) ;
#2066 = LINE ( 'NONE', #785, #13594 ) ;
#2067 = FACE_OUTER_BOUND ( 'NONE', #12399, .T. ) ;
#2068 = CARTESIAN_POINT ( 'NONE',  ( -3.750000000000007550, -6.495190528383289141, 0.000000000000000000 ) ) ;
#2069 = CARTESIAN_POINT ( 'NONE',  ( -1.846868145590734756, -29.37500000136559564, -4.458734124999999437 ) ) ;
#2070 = CARTESIAN_POINT ( 'NONE',  ( -4.276409079477644148, -1.261996585732578335, -0.8124999986344055847 ) ) ;
#2071 = VERTEX_POINT ( 'NONE', #4724 ) ;
#2072 = DIRECTION ( 'NONE',  ( -0.000000000000000000, -1.000000000000000000, -0.000000000000000000 ) ) ;
#2073 = ORIENTED_EDGE ( 'NONE', *, *, #7225, .F. ) ;
#2074 = VERTEX_POINT ( 'NONE', #5863 ) ;
#2075 = ORIENTED_EDGE ( 'NONE', *, *, #11616, .F. ) ;
#2076 = CARTESIAN_POINT ( 'NONE',  ( -1.846868145590737420, -29.00000000136559564, 4.458734124999999437 ) ) ;
#2077 = CARTESIAN_POINT ( 'NONE',  ( 0.000000000000000000, -20.00000000000000000, 5.000000000000000000 ) ) ;
#2078 = CARTESIAN_POINT ( 'NONE',  ( 0.000000000000000000, 40.00000000000000000, -57.99999999999999289 ) ) ;
#2079 = EDGE_CURVE ( 'NONE', #7857, #3918, #14581, .T. ) ;
#2080 = CARTESIAN_POINT ( 'NONE',  ( 0.5093500532425063732, 4.799145180956616130, -4.124999998634405252 ) ) ;
#2081 = CYLINDRICAL_SURFACE ( 'NONE', #8849, 2.649999999999992806 ) ;
#2082 = ADVANCED_FACE ( 'NONE', ( #13358 ), #2300, .T. ) ;
#2083 = ADVANCED_FACE ( 'NONE', ( #12146 ), #6102, .F. ) ;
#2084 = CARTESIAN_POINT ( 'NONE',  ( -114.9999999999999858, -109.4337567297407219, -17.50000000000000000 ) ) ;
#2085 = CARTESIAN_POINT ( 'NONE',  ( -4.799145180956616130, 0.5093500532425063732, -5.874999998634406140 ) ) ;
#2086 = CARTESIAN_POINT ( 'NONE',  ( -5.000000000000000888, -21.56250000273118772, 2.071067811865474617 ) ) ;
#2087 = DIRECTION ( 'NONE',  ( 0.000000000000000000, 0.000000000000000000, 1.000000000000000000 ) ) ;
#2088 = CARTESIAN_POINT ( 'NONE',  ( -1.846868145590737420, -30.75000000136559564, 4.458734124999999437 ) ) ;
#2089 = EDGE_LOOP ( 'NONE', ( #1432, #8925, #11103, #12155 ) ) ;
#2090 = CARTESIAN_POINT ( 'NONE',  ( -3.152801135295367985, -23.81250000136559564, 3.152801135295367096 ) ) ;
#2091 = DIRECTION ( 'NONE',  ( 0.000000000000000000, 0.000000000000000000, -1.000000000000000000 ) ) ;
#2092 = ORIENTED_EDGE ( 'NONE', *, *, #908, .F. ) ;
#2093 = ORIENTED_EDGE ( 'NONE', *, *, #14991, .F. ) ;
#2094 = DIRECTION ( 'NONE',  ( 0.000000000000000000, -1.000000000000000000, 0.000000000000000000 ) ) ;
#2095 = CARTESIAN_POINT ( 'NONE',  ( -1.846868145590737420, -30.75000000136559564, 4.458734124999999437 ) ) ;
#2096 = FACE_OUTER_BOUND ( 'NONE', #1526, .T. ) ;
#2097 = EDGE_LOOP ( 'NONE', ( #14132, #2475, #14126, #343 ) ) ;
#2098 = CARTESIAN_POINT ( 'NONE',  ( 5.000000000000004441, 3.034671531081452754E-15, -0.04526304759294640795 ) ) ;
#2099 = CARTESIAN_POINT ( 'NONE',  ( -44.99999999999999289, -35.00000000000000000, 17.50000000000000000 ) ) ;
#2100 = FACE_OUTER_BOUND ( 'NONE', #15094, .T. ) ;
#2101 = B_SPLINE_CURVE_WITH_KNOTS ( 'NONE', 3,
 ( #12103, #893, #12174, #4758, #10981 ),
 .UNSPECIFIED., .F., .F.,
 ( 4, 1, 4 ),
 ( 0.000000000000000000, 0.002309401076758505790, 0.004618802153517011580 ),
 .UNSPECIFIED. ) ;
#2102 = EDGE_CURVE ( 'NONE', #12678, #12016, #8834, .T. ) ;
#2103 = CARTESIAN_POINT ( 'NONE',  ( 4.458734124999999437, -26.75000000136559564, 1.846868145590737864 ) ) ;
#2104 = FACE_OUTER_BOUND ( 'NONE', #6226, .T. ) ;
#2105 = DIRECTION ( 'NONE',  ( 0.8660254037844388186, 0.000000000000000000, -0.4999999999999996669 ) ) ;
#2106 = CARTESIAN_POINT ( 'NONE',  ( 3.535533905932738197, -31.00000000273118772, -3.535533905932738197 ) ) ;
#2107 = DIRECTION ( 'NONE',  ( 0.5000000000000002220, -0.000000000000000000, -0.8660254037844384856 ) ) ;
#2108 = ORIENTED_EDGE ( 'NONE', *, *, #3126, .T. ) ;
#2109 = ORIENTED_EDGE ( 'NONE', *, *, #5990, .T. ) ;
#2110 = LINE ( 'NONE', #13174, #13653 ) ;
#2111 = ORIENTED_EDGE ( 'NONE', *, *, #14976, .F. ) ;
#2112 = EDGE_CURVE ( 'NONE', #14535, #8138, #5437, .T. ) ;
#2113 = DIRECTION ( 'NONE',  ( -1.000000000000000000, -0.000000000000000000, -0.000000000000000000 ) ) ;
#2114 = DIRECTION ( 'NONE',  ( 1.000000000000000000, 0.000000000000000000, 0.000000000000000000 ) ) ;
#2115 = CARTESIAN_POINT ( 'NONE',  ( 3.033343224707661712, -3.753672977998669946, -0.4999999986344072500 ) ) ;
#2116 = DIRECTION ( 'NONE',  ( 6.123233995736766036E-17, 1.000000000000000000, 0.000000000000000000 ) ) ;
#2117 = CARTESIAN_POINT ( 'NONE',  ( -3.033343224707664376, 3.753672977998667726, -0.2499999986344070280 ) ) ;
#2118 = CARTESIAN_POINT ( 'NONE',  ( 2.071067811865503927, -21.93750000273119127, -4.999999999999971578 ) ) ;
#2119 = VERTEX_POINT ( 'NONE', #12763 ) ;
#2120 = CARTESIAN_POINT ( 'NONE',  ( -5.000000000000000888, -22.56250000000000000, -2.071067811865475949 ) ) ;
#2121 = VERTEX_POINT ( 'NONE', #1708 ) ;
#2122 = DIRECTION ( 'NONE',  ( -0.000000000000000000, -1.000000000000000000, -0.000000000000000000 ) ) ;
#2123 = VERTEX_POINT ( 'NONE', #8918 ) ;
#2124 = AXIS2_PLACEMENT_3D ( 'NONE', #11950, #9545, #14472 ) ;
#2125 = ORIENTED_EDGE ( 'NONE', *, *, #10428, .T. ) ;
#2126 = CARTESIAN_POINT ( 'NONE',  ( 3.535533905932736864, -23.25000000273118772, 3.535533905932738641 ) ) ;
#2127 = EDGE_CURVE ( 'NONE', #9146, #13099, #2187, .T. ) ;
#2128 = CARTESIAN_POINT ( 'NONE',  ( 0.000000000000000000, 2.000000000000001776, 0.000000000000000000 ) ) ;
#2129 = CIRCLE ( 'NONE', #11669, 2.649999999999985700 ) ;
#2130 = ADVANCED_FACE ( 'NONE', ( #1861 ), #11638, .T. ) ;
#2131 = SURFACE_STYLE_USAGE ( .BOTH. , #1080 ) ;
#2132 = AXIS2_PLACEMENT_3D ( 'NONE', #8014, #9139, #11311 ) ;
#2133 = AXIS2_PLACEMENT_3D ( 'NONE', #13779, #2714, #472 ) ;
#2134 = CARTESIAN_POINT ( 'NONE',  ( -50.51988060489983212, 0.000000000000000000, 62.50099999999999767 ) ) ;
#2135 = DIRECTION ( 'NONE',  ( -0.000000000000000000, -1.000000000000000000, -0.000000000000000000 ) ) ;
#2136 = CARTESIAN_POINT ( 'NONE',  ( 35.00000000000000000, 37.00000000000000000, -8.572527594031472993E-15 ) ) ;
#2137 = AXIS2_PLACEMENT_3D ( 'NONE', #8660, #91, #4858 ) ;
#2138 = CARTESIAN_POINT ( 'NONE',  ( 4.391654775818395251, -2.390265326283149694, -0.9999999972688140559 ) ) ;
#2139 = CARTESIAN_POINT ( 'NONE',  ( 7.347880794884120722E-16, -11.00000000000000178, 6.000000000000000888 ) ) ;
#2140 = CARTESIAN_POINT ( 'NONE',  ( -17.99999999999979394, -9.000000000000001776, -3.500000000000000888 ) ) ;
#2141 = CARTESIAN_POINT ( 'NONE',  ( -8.190561711645485556E-16, -29.93750000136559564, 4.458734124999999437 ) ) ;
#2142 = CARTESIAN_POINT ( 'NONE',  ( 2.131511515620586383, 3.916244202832140253, -2.187499998634407028 ) ) ;
#2143 = VERTEX_POINT ( 'NONE', #10368 ) ;
#2144 = DIRECTION ( 'NONE',  ( 0.000000000000000000, 0.000000000000000000, -1.000000000000000000 ) ) ;
#2145 = ORIENTED_EDGE ( 'NONE', *, *, #10019, .T. ) ;
#2146 = EDGE_LOOP ( 'NONE', ( #849, #3533 ) ) ;
#2147 = EDGE_LOOP ( 'NONE', ( #8319, #4838, #7537, #3603 ) ) ;
#2148 = PRODUCT_DEFINITION_SHAPE ( 'NONE', 'NONE',  #15969 ) ;
#2149 = VECTOR ( 'NONE', #15502, 1000.000000000000000 ) ;
#2150 = CARTESIAN_POINT ( 'NONE',  ( 1.846868145590736310, -28.87500000136559564, 4.458734124999999437 ) ) ;
#2151 = DIRECTION ( 'NONE',  ( -0.000000000000000000, -1.000000000000000000, -0.000000000000000000 ) ) ;
#2152 = EDGE_CURVE ( 'NONE', #4793, #7552, #14824, .T. ) ;
#2153 = PRODUCT_DEFINITION ( 'UNKNOWN', '', #5085, #2371 ) ;
#2154 = CARTESIAN_POINT ( 'NONE',  ( -35.00000000000000000, 40.00000000000000000, -2.649999999999992806 ) ) ;
#2155 = LINE ( 'NONE', #12005, #190 ) ;
#2156 = DIRECTION ( 'NONE',  ( -0.8660254037844388186, 0.000000000000000000, 0.4999999999999997224 ) ) ;
#2157 = DIRECTION ( 'NONE',  ( 1.000000000000000000, 0.000000000000000000, 0.000000000000000000 ) ) ;
#2158 = CARTESIAN_POINT ( 'NONE',  ( -3.753672977998669946, -3.033343224707661712, -7.749999998634409692 ) ) ;
#2159 = DIRECTION ( 'NONE',  ( 0.000000000000000000, 1.000000000000000000, 0.000000000000000000 ) ) ;
#2160 = CARTESIAN_POINT ( 'NONE',  ( -2.086913300611921596, -4.342183829375121817, -0.1328488020282359572 ) ) ;
#2161 = CARTESIAN_POINT ( 'NONE',  ( 3.535533905932736864, -22.25000000273118417, 3.535533905932738641 ) ) ;
#2162 = ORIENTED_EDGE ( 'NONE', *, *, #14228, .T. ) ;
#2163 =( REPRESENTATION_RELATIONSHIP ('NONE','NONE', #4176, #15130 ) REPRESENTATION_RELATIONSHIP_WITH_TRANSFORMATION ( #8112 )SHAPE_REPRESENTATION_RELATIONSHIP( ) );
#2164 = FACE_BOUND ( 'NONE', #10857, .T. ) ;
#2165 = ORIENTED_EDGE ( 'NONE', *, *, #5262, .T. ) ;
#2166 = EDGE_LOOP ( 'NONE', ( #10473, #8805 ) ) ;
#2167 = CARTESIAN_POINT ( 'NONE',  ( -7.500000000000003553, -0.7729939684939154398, -7.026407045654484484 ) ) ;
#2168 = PRESENTATION_LAYER_ASSIGNMENT (  '', '', ( #8632 ) ) ;
#2169 = CARTESIAN_POINT ( 'NONE',  ( -4.458734124999999437, -28.93750000136559564, -5.460374474430324690E-16 ) ) ;
#2170 = ADVANCED_FACE ( 'NONE', ( #13821 ), #354, .F. ) ;
#2171 = CARTESIAN_POINT ( 'NONE',  ( 19.99999999999956657, -8.786575603324269439E-13, -13.00000000000000000 ) ) ;
#2172 = EDGE_CURVE ( 'NONE', #5460, #928, #5592, .T. ) ;
#2173 = AXIS2_PLACEMENT_3D ( 'NONE', #11228, #9857, #14789 ) ;
#2174 = ORIENTED_EDGE ( 'NONE', *, *, #2044, .T. ) ;
#2175 = CARTESIAN_POINT ( 'NONE',  ( 0.000000000000000000, 0.000000000000000000, 4.000000000000000000 ) ) ;
#2176 = CARTESIAN_POINT ( 'NONE',  ( 39.73946572741719052, -3.978804951770217091, -28.28016224734468409 ) ) ;
#2177 = CARTESIAN_POINT ( 'NONE',  ( -3.152801135295367096, -24.31250000136559564, -3.152801135295367541 ) ) ;
#2178 = STYLED_ITEM ( 'NONE', ( #5790 ), #7752 ) ;
#2179 = DIRECTION ( 'NONE',  ( -0.5000000000000002220, 0.000000000000000000, 0.8660254037844384856 ) ) ;
#2180 = DIRECTION ( 'NONE',  ( 0.000000000000000000, 0.000000000000000000, 1.000000000000000000 ) ) ;
#2181 = DIRECTION ( 'NONE',  ( -0.000000000000000000, 1.000000000000000000, -0.000000000000000000 ) ) ;
#2182 = CIRCLE ( 'NONE', #15101, 2.700000000000000622 ) ;
#2183 = CARTESIAN_POINT ( 'NONE',  ( -4.211140560182196957, -2.431303136016552013, -3.745885042887436178 ) ) ;
#2184 = ORIENTED_EDGE ( 'NONE', *, *, #11259, .T. ) ;
#2185 = ORIENTED_EDGE ( 'NONE', *, *, #5449, .T. ) ;
#2186 = CARTESIAN_POINT ( 'NONE',  ( -2.558993250143184461, 7.638875775590766359, -7.593821156097443570 ) ) ;
#2187 =( BOUNDED_CURVE ( )  B_SPLINE_CURVE ( 2, ( #12609, #6654, #11564, #3000, #11713, #11403, #9238, #8033, #15127, #1551, #12850 ),
 .UNSPECIFIED., .F., .F. ) 
 B_SPLINE_CURVE_WITH_KNOTS ( ( 3, 2, 2, 2, 2, 3 ),
 ( 0.7545872658012773293, 0.7624999999999999556, 0.7750000000000000222, 0.7874999999999999778, 0.8000000000000000444, 0.8045872658012773737 ),
 .UNSPECIFIED. ) 
 CURVE ( )  GEOMETRIC_REPRESENTATION_ITEM ( )  RATIONAL_B_SPLINE_CURVE ( ( 0.9646335149384803742, 0.9518143178943441196, 1.000000000000000000, 0.9238795325112867385, 1.000000000000000000, 0.9238795325112867385, 1.000000000000000000, 0.9238795325112867385, 1.000000000000000000, 0.9720652146169423968, 0.9646335149384803742 ) ) 
 REPRESENTATION_ITEM ( '' )  );
#2188 = EDGE_CURVE ( 'NONE', #15092, #15644, #6807, .T. ) ;
#2189 = AXIS2_PLACEMENT_3D ( 'NONE', #687, #5615, #1130 ) ;
#2190 = VERTEX_POINT ( 'NONE', #14165 ) ;
#2191 = VECTOR ( 'NONE', #9728, 1000.000000000000000 ) ;
#2192 = CARTESIAN_POINT ( 'NONE',  ( 0.000000000000000000, 0.000000000000000000, 0.000000000000000000 ) ) ;
#2193 = CARTESIAN_POINT ( 'NONE',  ( 40.11295108777448348, -3.387975324183181591, 27.90213124783379328 ) ) ;
#2194 = CARTESIAN_POINT ( 'NONE',  ( -2.131511515620587272, -3.916244202832140253, -0.6874999986344054737 ) ) ;
#2195 = DIRECTION ( 'NONE',  ( 6.123233995736766036E-17, 1.000000000000000000, 0.000000000000000000 ) ) ;
#2196 = VECTOR ( 'NONE', #11552, 1000.000000000000000 ) ;
#2197 = CARTESIAN_POINT ( 'NONE',  ( -4.799145180956616130, 0.5093500532425063732, -3.124999998634407916 ) ) ;
#2198 = CYLINDRICAL_SURFACE ( 'NONE', #694, 75.00000000000001421 ) ;
#2199 =( LENGTH_UNIT ( ) NAMED_UNIT ( * ) SI_UNIT ( .MILLI., .METRE. ) );
#2200 = VERTEX_POINT ( 'NONE', #10441 ) ;
#2201 = CARTESIAN_POINT ( 'NONE',  ( 2.500000000000000444, 0.000000000000000000, -5.000000000000000888 ) ) ;
#2202 = AXIS2_PLACEMENT_3D ( 'NONE', #14543, #3463, #3788 ) ;
#2203 = SURFACE_STYLE_FILL_AREA ( #14189 ) ;
#2204 = ORIENTED_EDGE ( 'NONE', *, *, #4643, .T. ) ;
#2205 = DIRECTION ( 'NONE',  ( -1.000000000000000000, -0.000000000000000000, -0.000000000000000000 ) ) ;
#2206 = EDGE_LOOP ( 'NONE', ( #7820, #14661, #10147, #6463, #13439 ) ) ;
#2207 = ORIENTED_EDGE ( 'NONE', *, *, #9075, .T. ) ;
#2208 = CARTESIAN_POINT ( 'NONE',  ( -4.799145180956616130, 0.5093500532425063732, -3.124999998634407472 ) ) ;
#2209 = CONICAL_SURFACE ( 'NONE', #8183, 4.000000000000000000, 0.8911886515913786111 ) ;
#2210 = CARTESIAN_POINT ( 'NONE',  ( 21.99999999999956657, -8.786575603324269439E-13, -4.500000000000000000 ) ) ;
#2211 = TOROIDAL_SURFACE ( 'NONE', #11252, 5.384454397937118664, 0.5155456020628804703 ) ;
#2212 = DIRECTION ( 'NONE',  ( 0.000000000000000000, 1.000000000000000000, 0.000000000000000000 ) ) ;
#2213 = CARTESIAN_POINT ( 'NONE',  ( 67.49999999999931788, 37.00000000000000000, 2.081668171172168513E-14 ) ) ;
#2214 = CARTESIAN_POINT ( 'NONE',  ( -9.184850993605147944E-16, -29.37500000273118417, 5.000000000000000000 ) ) ;
#2215 = CARTESIAN_POINT ( 'NONE',  ( 4.795541693661363958, 1.415196051561583790, 1.125000002731184390 ) ) ;
#2216 = CARTESIAN_POINT ( 'NONE',  ( -9.184850993605147944E-16, -24.25000000000000000, 5.000000000000000000 ) ) ;
#2217 = EDGE_CURVE ( 'NONE', #14425, #7414, #5929, .T. ) ;
#2218 = CARTESIAN_POINT ( 'NONE',  ( 4.458734124999999437, -29.62500000136559208, -1.846868145590734978 ) ) ;
#2219 = CARTESIAN_POINT ( 'NONE',  ( 2.131511515620586383, 3.916244202832140253, -4.187499998634405252 ) ) ;
#2220 = VERTEX_POINT ( 'NONE', #14073 ) ;
#2221 = CARTESIAN_POINT ( 'NONE',  ( -0.04725809328185331254, 9.175759667312515688, -8.057670357645360326 ) ) ;
#2222 = ORIENTED_EDGE ( 'NONE', *, *, #1236, .F. ) ;
#2223 = ORIENTED_EDGE ( 'NONE', *, *, #7879, .T. ) ;
#2224 = CIRCLE ( 'NONE', #11263, 2.500000000000909495 ) ;
#2225 = SURFACE_SIDE_STYLE ('',( #7097 ) ) ;
#2226 = EDGE_LOOP ( 'NONE', ( #14757, #13715, #10358, #5017 ) ) ;
#2227 = CARTESIAN_POINT ( 'NONE',  ( 3.152801135295367541, -27.56250000136559564, -3.152801135295367541 ) ) ;
#2228 = DIRECTION ( 'NONE',  ( 0.4999999999999997224, 0.000000000000000000, 0.8660254037844387076 ) ) ;
#2229 = FACE_OUTER_BOUND ( 'NONE', #11324, .T. ) ;
#2230 = AXIS2_PLACEMENT_3D ( 'NONE', #8871, #9906, #8713 ) ;
#2231 = CARTESIAN_POINT ( 'NONE',  ( -21.01110699893060030, 2.000000000000000000, 36.39230484541324273 ) ) ;
#2232 = CARTESIAN_POINT ( 'NONE',  ( 4.472333508125966972, -3.761076017575723629, 48.59513319789044772 ) ) ;
#2233 = CARTESIAN_POINT ( 'NONE',  ( 2.521252210804794114, -4.248023353278823855, -0.04711480227235904233 ) ) ;
#2234 = VECTOR ( 'NONE', #10201, 1000.000000000000000 ) ;
#2235 = DIRECTION ( 'NONE',  ( -0.000000000000000000, -1.000000000000000000, -0.000000000000000000 ) ) ;
#2236 = CARTESIAN_POINT ( 'NONE',  ( 4.209348295687701302, 3.401574460001765665, -2.937500000000003109 ) ) ;
#2237 = CARTESIAN_POINT ( 'NONE',  ( -5.000000000000000888, 6.123233995736767268E-16, -9.999999999999998224 ) ) ;
#2238 = EDGE_CURVE ( 'NONE', #12516, #1307, #11996, .T. ) ;
#2239 = CARTESIAN_POINT ( 'NONE',  ( 10.00000000000098765, -13.00000000000000178, 14.82050807568871065 ) ) ;
#2240 = ADVANCED_FACE ( 'NONE', ( #12115 ), #4615, .T. ) ;
#2241 = CARTESIAN_POINT ( 'NONE',  ( 4.458734124999999437, -29.43750000136559208, 0.000000000000000000 ) ) ;
#2242 = CARTESIAN_POINT ( 'NONE',  ( -2.131511515620587272, -3.916244202832140253, 1.062500001365592528 ) ) ;
#2243 = VERTEX_POINT ( 'NONE', #15539 ) ;
#2244 = CARTESIAN_POINT ( 'NONE',  ( 2.500000000000000000, 0.000000000000000000, 0.000000000000000000 ) ) ;
#2245 = EDGE_LOOP ( 'NONE', ( #692, #3137, #868, #3826 ) ) ;
#2246 = AXIS2_PLACEMENT_3D ( 'NONE', #935, #5861, #4648 ) ;
#2247 = VERTEX_POINT ( 'NONE', #1943 ) ;
#2248 = CARTESIAN_POINT ( 'NONE',  ( -7.908219015560236542, -3.084967917786102465, -7.795665562178456298 ) ) ;
#2249 = CARTESIAN_POINT ( 'NONE',  ( 4.458734124999999437, -30.43750000136559564, 0.000000000000000000 ) ) ;
#2250 = LINE ( 'NONE', #8497, #12002 ) ;
#2251 = ORIENTED_EDGE ( 'NONE', *, *, #8326, .F. ) ;
#2252 = AXIS2_PLACEMENT_3D ( 'NONE', #12708, #1648, #5213 ) ;
#2253 = FACE_OUTER_BOUND ( 'NONE', #9899, .T. ) ;
#2255 = AXIS2_PLACEMENT_3D ( 'NONE', #2576, #7849, #2655 ) ;
#2254 = DIRECTION ( 'NONE',  ( 0.000000000000000000, 0.000000000000000000, 1.000000000000000000 ) ) ;
#2256 = SPHERICAL_SURFACE ( 'NONE', #9506, 10.00000000000000000 ) ;
#2257 = DIRECTION ( 'NONE',  ( -1.000000000000000000, 0.000000000000000000, 0.000000000000000000 ) ) ;
#2258 = AXIS2_PLACEMENT_3D ( 'NONE', #10852, #15792, #7303 ) ;
#2259 = CARTESIAN_POINT ( 'NONE',  ( 4.458734124999999437, -22.68750000136559564, 0.000000000000000000 ) ) ;
#2260 = CARTESIAN_POINT ( 'NONE',  ( 35.00000000000000000, 40.00000000000000000, 0.000000000000000000 ) ) ;
#2261 = EDGE_CURVE ( 'NONE', #2143, #2783, #3919, .T. ) ;
#2262 = DIRECTION ( 'NONE',  ( 0.000000000000000000, 0.000000000000000000, -1.000000000000000000 ) ) ;
#2263 = ADVANCED_FACE ( 'NONE', ( #5824 ), #1079, .F. ) ;
#2264 =( NAMED_UNIT ( * ) SI_UNIT ( $, .STERADIAN. ) SOLID_ANGLE_UNIT ( ) );
#2265 = DIRECTION ( 'NONE',  ( 1.000000000000000000, 0.000000000000000000, 0.000000000000000000 ) ) ;
#2266 = CARTESIAN_POINT ( 'NONE',  ( 5.000000000000002665, 3.306546357697854226E-16, 2.700000000000001066 ) ) ;
#2267 = EDGE_LOOP ( 'NONE', ( #922, #2540, #10016 ) ) ;
#2268 = SURFACE_SIDE_STYLE ('',( #7456 ) ) ;
#2269 = MECHANICAL_DESIGN_GEOMETRIC_PRESENTATION_REPRESENTATION (  '', ( #9256 ), #10548 ) ;
#2270 = EDGE_LOOP ( 'NONE', ( #10617, #3870, #9843, #1976 ) ) ;
#2271 = FACE_OUTER_BOUND ( 'NONE', #5958, .T. ) ;
#2272 = AXIS2_PLACEMENT_3D ( 'NONE', #3749, #8697, #7653 ) ;
#2273 = VERTEX_POINT ( 'NONE', #5913 ) ;
#2274 = CIRCLE ( 'NONE', #11563, 57.99999999999999289 ) ;
#2275 = CARTESIAN_POINT ( 'NONE',  ( -3.535533905932738641, -26.37500000000000355, 3.535533905932737309 ) ) ;
#2276 = FACE_BOUND ( 'NONE', #7389, .T. ) ;
#2277 = ADVANCED_FACE ( 'NONE', ( #2104 ), #14474, .F. ) ;
#2278 = CARTESIAN_POINT ( 'NONE',  ( -1.261996585732579224, 4.276409079477648589, -1.062499998634405696 ) ) ;
#2279 = VECTOR ( 'NONE', #1746, 1000.000000000000114 ) ;
#2280 = DIRECTION ( 'NONE',  ( 0.000000000000000000, 0.000000000000000000, 1.000000000000000000 ) ) ;
#2281 = EDGE_CURVE ( 'NONE', #15345, #10675, #14755, .T. ) ;
#2282 = PRODUCT ( 'pin', 'pin', '', ( #8596 ) ) ;
#2283 = CARTESIAN_POINT ( 'NONE',  ( 3.033343224707661712, -3.753672977998669946, -1.749999998634408360 ) ) ;
#2284 = DIRECTION ( 'NONE',  ( -0.000000000000000000, 1.000000000000000000, -0.000000000000000000 ) ) ;
#2285 = CARTESIAN_POINT ( 'NONE',  ( 3.061616997868383141E-16, -21.87500000273118772, -4.999999999999999112 ) ) ;
#2286 = EDGE_LOOP ( 'NONE', ( #1437, #8006, #10768, #7115, #2904, #11120, #4080, #10979 ) ) ;
#2287 = DIRECTION ( 'NONE',  ( -1.000000000000000000, -0.000000000000000000, -0.000000000000000000 ) ) ;
#2288 = CONICAL_SURFACE ( 'NONE', #11326, 2.055000000000000160, 0.7853981633974633780 ) ;
#2289 =( NAMED_UNIT ( * ) PLANE_ANGLE_UNIT ( ) SI_UNIT ( $, .RADIAN. ) );
#2290 = ORIENTED_EDGE ( 'NONE', *, *, #12191, .F. ) ;
#2291 = CYLINDRICAL_SURFACE ( 'NONE', #7229, 30.00000000000000711 ) ;
#2292 = VERTEX_POINT ( 'NONE', #7214 ) ;
#2293 = EDGE_LOOP ( 'NONE', ( #12874, #3623, #1545, #4562 ) ) ;
#2294 = CARTESIAN_POINT ( 'NONE',  ( 1.261996585732578113, -4.276409079477644148, -3.812499998634408360 ) ) ;
#2295 = VECTOR ( 'NONE', #11312, 1000.000000000000000 ) ;
#2296 = CIRCLE ( 'NONE', #1009, 10.12668159690567649 ) ;
#2297 = LINE ( 'NONE', #3424, #6588 ) ;
#2298 = CARTESIAN_POINT ( 'NONE',  ( -2.345747346278108214, 3.264484291692489215, -0.01223254789873409049 ) ) ;
#2299 = CARTESIAN_POINT ( 'NONE',  ( 5.200000000000002842, 0.000000000000000000, 2.500000000000000444 ) ) ;
#2300 = PLANE ( 'NONE',  #7028 ) ;
#2301 = EDGE_CURVE ( 'NONE', #13811, #7787, #12940, .T. ) ;
#2302 = CARTESIAN_POINT ( 'NONE',  ( -2.071067811865489272, -29.81250000273117706, -4.999999999999985789 ) ) ;
#2303 = CARTESIAN_POINT ( 'NONE',  ( 4.209348295687701302, 3.401574460001765665, -1.812499997268814278 ) ) ;
#2304 = CARTESIAN_POINT ( 'NONE',  ( -5.000000000000000888, -24.56250000000000000, -2.071067811865475949 ) ) ;
#2305 = CARTESIAN_POINT ( 'NONE',  ( -3.535533905932737309, -22.75000000273118772, -3.535533905932738197 ) ) ;
#2306 = CARTESIAN_POINT ( 'NONE',  ( 4.458734124999997661, -25.75000000136559564, 1.846868145590737864 ) ) ;
#2307 = CARTESIAN_POINT ( 'NONE',  ( -1.261996585732579224, 4.276409079477648589, -3.062499998634407472 ) ) ;
#2308 = AXIS2_PLACEMENT_3D ( 'NONE', #7872, #8843, #13748 ) ;
#2309 = CARTESIAN_POINT ( 'NONE',  ( -43.85680617780057844, -3.000000000000000000, 22.00000000000000355 ) ) ;
#2310 = ORIENTED_EDGE ( 'NONE', *, *, #11766, .T. ) ;
#2311 = EDGE_LOOP ( 'NONE', ( #5185, #10664, #326, #13860 ) ) ;
#2312 = ORIENTED_EDGE ( 'NONE', *, *, #383, .T. ) ;
#2313 = CARTESIAN_POINT ( 'NONE',  ( 4.458734125000000326, -22.62500000136559564, -1.846868145590734978 ) ) ;
#2314 = CARTESIAN_POINT ( 'NONE',  ( -115.0000000000000142, -10.00000000000000888, 7.500000000000001776 ) ) ;
#2315 = CARTESIAN_POINT ( 'NONE',  ( -114.9999999999999858, -109.4337567297407219, -17.50000000000000000 ) ) ;
#2316 = EDGE_CURVE ( 'NONE', #2243, #9104, #9389, .T. ) ;
#2317 = LINE ( 'NONE', #3611, #13079 ) ;
#2318 = CYLINDRICAL_SURFACE ( 'NONE', #10138, 2.000000000000001776 ) ;
#2319 = CARTESIAN_POINT ( 'NONE',  ( -9.184850993605147944E-16, -22.25000000000000000, 5.000000000000000000 ) ) ;
#2320 = CARTESIAN_POINT ( 'NONE',  ( 4.795541693661363958, 1.415196051561583790, -3.469446951953614189E-15 ) ) ;
#2321 = LINE ( 'NONE', #14939, #15313 ) ;
#2322 = CARTESIAN_POINT ( 'NONE',  ( -2.071067811865463959, -27.31250000000000000, 5.000000000000013323 ) ) ;
#2323 = CARTESIAN_POINT ( 'NONE',  ( -4.458734125000001214, -24.87500000136559919, 1.846868145590734089 ) ) ;
#2324 = CARTESIAN_POINT ( 'NONE',  ( 3.033343224707661712, -3.753672977998669946, -0.7499999986344074721 ) ) ;
#2325 = EDGE_LOOP ( 'NONE', ( #4394, #13278, #3117, #12707, #15185, #9385, #5150, #12361, #3224, #6361 ) ) ;
#2326 = CARTESIAN_POINT ( 'NONE',  ( -9.184850993605147944E-16, -29.25000000000000000, 5.000000000000000000 ) ) ;
#2327 = ORIENTED_EDGE ( 'NONE', *, *, #13355, .F. ) ;
#2328 = VERTEX_POINT ( 'NONE', #3328 ) ;
#2329 = DIRECTION ( 'NONE',  ( 1.000000000000000000, 0.000000000000000000, -1.239088197126290570E-16 ) ) ;
#2330 = CARTESIAN_POINT ( 'NONE',  ( 3.152801135295366208, -23.56250000136559564, 3.152801135295367985 ) ) ;
#2331 = CARTESIAN_POINT ( 'NONE',  ( -9.184850993605147944E-16, -23.25000000000000000, 5.000000000000000000 ) ) ;
#2332 = ORIENTED_EDGE ( 'NONE', *, *, #12839, .T. ) ;
#2333 = FACE_BOUND ( 'NONE', #10709, .T. ) ;
#2334 = EDGE_CURVE ( 'NONE', #3131, #15817, #13089, .T. ) ;
#2335 = EDGE_CURVE ( 'NONE', #10748, #15162, #13193, .T. ) ;
#2336 = CARTESIAN_POINT ( 'NONE',  ( -39.99999999999999289, -11.00000000000000178, 8.300651832549021947E-13 ) ) ;
#2337 = CARTESIAN_POINT ( 'NONE',  ( 4.154306624731137099, 2.398490048084935822, -3.721999068284414847 ) ) ;
#2338 = LINE ( 'NONE', #1049, #4469 ) ;
#2339 = CARTESIAN_POINT ( 'NONE',  ( 1.846868145590736310, -24.87500000136559919, 4.458734124999999437 ) ) ;
#2340 = CARTESIAN_POINT ( 'NONE',  ( 0.000000000000000000, 0.000000000000000000, 0.000000000000000000 ) ) ;
#2341 = PLANE ( 'NONE',  #14956 ) ;
#2342 = CARTESIAN_POINT ( 'NONE',  ( 3.535533905932736864, -31.12500000000000000, 3.535533905932738641 ) ) ;
#2343 = LINE ( 'NONE', #3799, #14793 ) ;
#2344 = DIRECTION ( 'NONE',  ( 0.000000000000000000, -0.000000000000000000, -1.000000000000000000 ) ) ;
#2345 = FACE_BOUND ( 'NONE', #1530, .T. ) ;
#2346 = ORIENTED_EDGE ( 'NONE', *, *, #6446, .T. ) ;
#2347 = ORIENTED_EDGE ( 'NONE', *, *, #5359, .F. ) ;
#2348 = DIRECTION ( 'NONE',  ( -6.938893903907228378E-16, -1.000000000000000000, 0.000000000000000000 ) ) ;
#2349 = ORIENTED_EDGE ( 'NONE', *, *, #12452, .T. ) ;
#2350 = EDGE_CURVE ( 'NONE', #307, #2847, #1051, .T. ) ;
#2351 = CARTESIAN_POINT ( 'NONE',  ( 2.500000000000000000, 0.000000000000000000, 0.000000000000000000 ) ) ;
#2352 = DIRECTION ( 'NONE',  ( 0.5000000000000001110, 0.000000000000000000, -0.8660254037844384856 ) ) ;
#2353 = CARTESIAN_POINT ( 'NONE',  ( 5.000000000000000000, -28.00000000000000000, 0.000000000000000000 ) ) ;
#2354 = CARTESIAN_POINT ( 'NONE',  ( 10.00000000000001066, -13.50000000000000178, 17.32050807568925777 ) ) ;
#2355 = CARTESIAN_POINT ( 'NONE',  ( -3.753672977998669946, -3.033343224707661712, -1.999999998634408360 ) ) ;
#2356 = DIRECTION ( 'NONE',  ( 0.000000000000000000, -0.000000000000000000, -1.000000000000000000 ) ) ;
#2357 = CARTESIAN_POINT ( 'NONE',  ( 2.449848172108560096, 3.432307619358740514, -3.503702292528905637 ) ) ;
#2358 = CARTESIAN_POINT ( 'NONE',  ( 2.500000000000000000, 1.178949249685213863, -2.042000000000001148 ) ) ;
#2359 = EDGE_LOOP ( 'NONE', ( #6420, #458, #6480 ) ) ;
#2360 = CARTESIAN_POINT ( 'NONE',  ( 4.000000000000000000, -2.471525695159793035, -3.686886880705770864 ) ) ;
#2361 = CARTESIAN_POINT ( 'NONE',  ( 42.02221399786069611, 0.000000000000000000, 1.075528555105620399E-13 ) ) ;
#2362 = ORIENTED_EDGE ( 'NONE', *, *, #15794, .F. ) ;
#2363 = CARTESIAN_POINT ( 'NONE',  ( 3.916244202832140253, -2.131511515620588160, -3.687499998634407916 ) ) ;
#2364 = EDGE_CURVE ( 'NONE', #5212, #2989, #11952, .T. ) ;
#2365 = EDGE_CURVE ( 'NONE', #9517, #7038, #8277, .T. ) ;
#2366 = ADVANCED_FACE ( 'NONE', ( #749 ), #6545, .F. ) ;
#2367 = CARTESIAN_POINT ( 'NONE',  ( 0.000000000000000000, 1.178949249685218525, 2.041999999999999371 ) ) ;
#2368 = CYLINDRICAL_SURFACE ( 'NONE', #3075, 5.000000000000000888 ) ;
#2369 = LINE ( 'NONE', #5776, #15154 ) ;
#2370 = DIRECTION ( 'NONE',  ( -1.982541115402065110E-16, 1.000000000000000000, 0.000000000000000000 ) ) ;
#2371 = PRODUCT_DEFINITION_CONTEXT ( 'detailed design', #7449, 'design' ) ;
#2372 = CARTESIAN_POINT ( 'NONE',  ( 6.000000000000000000, -20.00000000000000000, -1.500000000000000000 ) ) ;
#2373 = CARTESIAN_POINT ( 'NONE',  ( -5.381735091635034607, 0.5711823568785950878, 0.5625000027311820583 ) ) ;
#2374 = CARTESIAN_POINT ( 'NONE',  ( 3.152801135295366208, -26.81250000136559564, 3.152801135295367985 ) ) ;
#2375 = DIRECTION ( 'NONE',  ( -0.000000000000000000, -1.000000000000000000, -0.000000000000000000 ) ) ;
#2376 = CARTESIAN_POINT ( 'NONE',  ( -4.276409079477644148, -1.261996585732578335, -4.812499998634405252 ) ) ;
#2377 = FACE_OUTER_BOUND ( 'NONE', #6162, .T. ) ;
#2378 = ORIENTED_EDGE ( 'NONE', *, *, #10013, .T. ) ;
#2379 = VERTEX_POINT ( 'NONE', #14713 ) ;
#2380 = CARTESIAN_POINT ( 'NONE',  ( 0.000000000000000000, 0.000000000000000000, 0.000000000000000000 ) ) ;
#2381 = VERTEX_POINT ( 'NONE', #13721 ) ;
#2382 = CARTESIAN_POINT ( 'NONE',  ( 3.152801135295367541, -24.56250000136559564, -3.152801135295367541 ) ) ;
#2383 = DIRECTION ( 'NONE',  ( 1.000000000000000000, 0.000000000000000000, 0.000000000000000000 ) ) ;
#2384 = ADVANCED_FACE ( 'NONE', ( #13402, #3636 ), #2654, .T. ) ;
#2385 = DIRECTION ( 'NONE',  ( 1.982541115402065110E-16, -1.000000000000000000, 0.000000000000000000 ) ) ;
#2386 = CARTESIAN_POINT ( 'NONE',  ( -67.50000000000000000, 50.00000000000000000, 2.649999999999278710 ) ) ;
#2387 = DIRECTION ( 'NONE',  ( -3.343241100358131282E-16, -0.000000000000000000, 1.000000000000000000 ) ) ;
#2388 = CARTESIAN_POINT ( 'NONE',  ( 2.071067811865476394, -22.18749999999999645, 5.000000000000000000 ) ) ;
#2389 = CARTESIAN_POINT ( 'NONE',  ( -4.391654775818395251, 2.390265326283148806, -0.6250000000000005551 ) ) ;
#2390 = LINE ( 'NONE', #2481, #3182 ) ;
#2391 = CARTESIAN_POINT ( 'NONE',  ( -4.678271028438514278, -0.2656286248631474223, -0.2252770511478082716 ) ) ;
#2392 = CARTESIAN_POINT ( 'NONE',  ( -8.190561711645485556E-16, -25.68750000136559564, 4.458734124999999437 ) ) ;
#2393 = CARTESIAN_POINT ( 'NONE',  ( -3.753672977998669946, -3.033343224707661712, -2.999999998634409248 ) ) ;
#2394 = ORIENTED_EDGE ( 'NONE', *, *, #9392, .F. ) ;
#2395 = CARTESIAN_POINT ( 'NONE',  ( 3.061616997868383141E-16, -30.87500000273118772, -5.000000000000000000 ) ) ;
#2396 = ORIENTED_EDGE ( 'NONE', *, *, #12301, .F. ) ;
#2397 = ORIENTED_EDGE ( 'NONE', *, *, #1296, .F. ) ;
#2398 = DIRECTION ( 'NONE',  ( -0.000000000000000000, 1.000000000000000000, -0.000000000000000000 ) ) ;
#2399 = CARTESIAN_POINT ( 'NONE',  ( 1.846868145590736310, -25.62500000136559564, 4.458734124999999437 ) ) ;
#2400 = LINE ( 'NONE', #12258, #3251 ) ;
#2401 = VERTEX_POINT ( 'NONE', #7526 ) ;
#2402 = DIRECTION ( 'NONE',  ( -0.000000000000000000, -1.000000000000000000, -0.000000000000000000 ) ) ;
#2403 = FACE_OUTER_BOUND ( 'NONE', #3347, .T. ) ;
#2404 = CYLINDRICAL_SURFACE ( 'NONE', #6157, 3.499999999999999556 ) ;
#2405 = DIRECTION ( 'NONE',  ( 0.000000000000000000, 0.000000000000000000, 1.000000000000000000 ) ) ;
#2406 = CARTESIAN_POINT ( 'NONE',  ( 5.000000000000000000, -32.00000000000000000, 0.000000000000000000 ) ) ;
#2407 = CARTESIAN_POINT ( 'NONE',  ( -9.184850993605147944E-16, -23.37500000273118772, 5.000000000000000000 ) ) ;
#2408 = CARTESIAN_POINT ( 'NONE',  ( -6.473970235329672780E-16, -4.862606272033106691, -3.745885042887442395 ) ) ;
#2409 = CARTESIAN_POINT ( 'NONE',  ( -5.000000000000000000, -29.62500000273118417, -6.123233995736766282E-16 ) ) ;
#2410 = CARTESIAN_POINT ( 'NONE',  ( 4.276409079477644148, 1.261996585732577891, -8.562499998634409692 ) ) ;
#2411 = CARTESIAN_POINT ( 'NONE',  ( 1.846868145590736310, -29.62500000136559208, 4.458734124999997661 ) ) ;
#2412 = EDGE_CURVE ( 'NONE', #12993, #5955, #6064, .T. ) ;
#2414 = EDGE_CURVE ( 'NONE', #13901, #3131, #8820, .T. ) ;
#2413 = ORIENTED_EDGE ( 'NONE', *, *, #14745, .T. ) ;
#2415 =( BOUNDED_CURVE ( )  B_SPLINE_CURVE ( 2, ( #14804, #11092, #11159, #2422, #15948, #9710, #4872, #9799, #10848 ),
 .UNSPECIFIED., .F., .F. ) 
 B_SPLINE_CURVE_WITH_KNOTS ( ( 3, 2, 2, 2, 3 ),
 ( 0.5250000000000001332, 0.5375000000000000888, 0.5500000000000002665, 0.5625000000000002220, 0.5750000000000001776 ),
 .UNSPECIFIED. ) 
 CURVE ( )  GEOMETRIC_REPRESENTATION_ITEM ( )  RATIONAL_B_SPLINE_CURVE ( ( 0.9999999999999993339, 0.9238795325112874046, 1.000000000000000000, 0.9238795325112867385, 1.000000000000000000, 0.9238795325112867385, 1.000000000000000000, 0.9238795325112854062, 1.000000000000001332 ) ) 
 REPRESENTATION_ITEM ( '' )  );
#2416 = ORIENTED_EDGE ( 'NONE', *, *, #8575, .F. ) ;
#2417 = CARTESIAN_POINT ( 'NONE',  ( -2.000000000000006661, 3.464101615137750834, 0.000000000000000000 ) ) ;
#2418 = EDGE_LOOP ( 'NONE', ( #3030, #5033 ) ) ;
#2419 = FACE_OUTER_BOUND ( 'NONE', #1069, .T. ) ;
#2420 = AXIS2_PLACEMENT_3D ( 'NONE', #7301, #8361, #12049 ) ;
#2421 = AXIS2_PLACEMENT_3D ( 'NONE', #2946, #7004, #779 ) ;
#2422 = CARTESIAN_POINT ( 'NONE',  ( -5.000000000000000888, -25.68750000273118772, -2.071067811865475949 ) ) ;
#2423 = CARTESIAN_POINT ( 'NONE',  ( 3.916244202832140253, -2.131511515620588160, -2.437499998634407028 ) ) ;
#2424 = SHAPE_DEFINITION_REPRESENTATION ( #11948, #279 ) ;
#2425 = CARTESIAN_POINT ( 'NONE',  ( 0.5093500532425063732, 4.799145180956616130, -1.374999998634406140 ) ) ;
#2426 = EDGE_CURVE ( 'NONE', #12637, #11426, #4770, .T. ) ;
#2427 = CARTESIAN_POINT ( 'NONE',  ( 3.535533905932736864, -24.12500000000000000, 3.535533905932738641 ) ) ;
#2428 = ADVANCED_FACE ( 'NONE', ( #3794, #3550 ), #12505, .T. ) ;
#2429 = MECHANICAL_DESIGN_GEOMETRIC_PRESENTATION_REPRESENTATION (  '', ( #141 ), #12276 ) ;
#2430 = CARTESIAN_POINT ( 'NONE',  ( 43.08845726811992449, 0.000000000000000000, -38.63139720814411504 ) ) ;
#2431 = AXIS2_PLACEMENT_3D ( 'NONE', #12948, #1885, #6826 ) ;
#2432 = SURFACE_STYLE_FILL_AREA ( #13492 ) ;
#2433 = VERTEX_POINT ( 'NONE', #2407 ) ;
#2434 = CARTESIAN_POINT ( 'NONE',  ( 4.000000000000000000, -1.700175430507292473, -3.320327275037661785 ) ) ;
#2435 = CARTESIAN_POINT ( 'NONE',  ( 10.00000000000098765, -20.00000000000000000, 17.32050807568871065 ) ) ;
#2436 = CIRCLE ( 'NONE', #3738, 0.2000000000000000944 ) ;
#2437 = ORIENTED_EDGE ( 'NONE', *, *, #520, .F. ) ;
#2438 = CARTESIAN_POINT ( 'NONE',  ( 3.753672977998667726, 3.033343224707664820, -2.499999998634408804 ) ) ;
#2439 = B_SPLINE_CURVE_WITH_KNOTS ( 'NONE', 3,
 ( #14004, #5287, #15068, #3985, #7738 ),
 .UNSPECIFIED., .F., .F.,
 ( 4, 1, 4 ),
 ( 5.640274452250024914E-20, 0.002309401076758505356, 0.004618802153517010713 ),
 .UNSPECIFIED. ) ;
#2440 = CARTESIAN_POINT ( 'NONE',  ( -3.355112389629170799, 2.681727112203152963, -0.2256878752776689534 ) ) ;
#2441 = FACE_OUTER_BOUND ( 'NONE', #3474, .T. ) ;
#2442 = CARTESIAN_POINT ( 'NONE',  ( -45.00000000000000000, 0.000000000000000000, -7.500000000000000000 ) ) ;
#2443 = AXIS2_PLACEMENT_3D ( 'NONE', #2666, #1546, #7617 ) ;
#2444 = CARTESIAN_POINT ( 'NONE',  ( -5.000000000000000888, -30.56250000273118772, 2.071067811865474617 ) ) ;
#2445 = CARTESIAN_POINT ( 'NONE',  ( -5.381735091635034607, 0.5711823568785950878, -0.4374999972688187744 ) ) ;
#2446 = CARTESIAN_POINT ( 'NONE',  ( 3.061616997868383141E-16, -24.75000000000000000, -5.000000000000000000 ) ) ;
#2447 = ADVANCED_FACE ( 'NONE', ( #4855 ), #9781, .T. ) ;
#2448 = CARTESIAN_POINT ( 'NONE',  ( 0.5789871446316211534, 4.420982230657665824, -0.3789984458506777676 ) ) ;
#2449 = CARTESIAN_POINT ( 'NONE',  ( -4.458734125000000326, -24.12500000136559919, 1.846868145590734089 ) ) ;
#2450 = EDGE_CURVE ( 'NONE', #10893, #1214, #15851, .T. ) ;
#2451 = CARTESIAN_POINT ( 'NONE',  ( -4.458734124999999437, -21.93750000136559208, -5.460374474430324690E-16 ) ) ;
#2452 = CARTESIAN_POINT ( 'NONE',  ( -4.799145180956616130, 0.5093500532425063732, -4.874999998634405252 ) ) ;
#2453 = CARTESIAN_POINT ( 'NONE',  ( 31.75426480542940766, -37.00000000000000711, 15.00000000000001066 ) ) ;
#2454 = VERTEX_POINT ( 'NONE', #9694 ) ;
#2455 = ORIENTED_EDGE ( 'NONE', *, *, #8323, .T. ) ;
#2456 = CONICAL_SURFACE ( 'NONE', #11001, 2.055000000000000160, 0.7853981633974721488 ) ;
#2457 = VERTEX_POINT ( 'NONE', #6311 ) ;
#2458 = CARTESIAN_POINT ( 'NONE',  ( 4.458734125000000326, -24.62500000136559564, -1.846868145590734978 ) ) ;
#2459 = DIRECTION ( 'NONE',  ( 0.8191520442889902442, 1.003171929053522651E-16, -0.5735764363510482688 ) ) ;
#2460 = FACE_OUTER_BOUND ( 'NONE', #13479, .T. ) ;
#2461 =( REPRESENTATION_RELATIONSHIP ('NONE','NONE', #4176, #7495 ) REPRESENTATION_RELATIONSHIP_WITH_TRANSFORMATION ( #15466 )SHAPE_REPRESENTATION_RELATIONSHIP( ) );
#2462 = DIRECTION ( 'NONE',  ( 0.000000000000000000, -0.000000000000000000, -1.000000000000000000 ) ) ;
#2463 = LINE ( 'NONE', #12241, #4705 ) ;
#2464 = CARTESIAN_POINT ( 'NONE',  ( -15.99999999999979217, -9.000000000000001776, -1.500000000000001110 ) ) ;
#2465 = CARTESIAN_POINT ( 'NONE',  ( -4.209348295687703967, -3.401574460001763001, -2.437500000000003109 ) ) ;
#2466 = DIRECTION ( 'NONE',  ( -1.000000000000000000, 0.000000000000000000, 0.000000000000000000 ) ) ;
#2467 = ADVANCED_FACE ( 'NONE', ( #14632, #8508 ), #7283, .F. ) ;
#2468 = CARTESIAN_POINT ( 'NONE',  ( 4.458734124999999437, -25.43750000136559564, 0.000000000000000000 ) ) ;
#2469 = AXIS2_PLACEMENT_3D ( 'NONE', #1218, #4942, #1300 ) ;
#2470 = ADVANCED_FACE ( 'NONE', ( #1208 ), #15864, .T. ) ;
#2471 = CARTESIAN_POINT ( 'NONE',  ( 3.753672977998667726, 3.033343224707664376, -3.499999998634410137 ) ) ;
#2472 = ORIENTED_EDGE ( 'NONE', *, *, #5941, .F. ) ;
#2473 = CARTESIAN_POINT ( 'NONE',  ( 45.58845726811988897, -5.000000000000000000, 42.96152422706632734 ) ) ;
#2474 = VERTEX_POINT ( 'NONE', #11146 ) ;
#2475 = ORIENTED_EDGE ( 'NONE', *, *, #3082, .T. ) ;
#2476 = CARTESIAN_POINT ( 'NONE',  ( 12.67949192431120586, -37.00000000000000711, 61.96152422706632024 ) ) ;
#2477 = CARTESIAN_POINT ( 'NONE',  ( -4.458734125000001214, -22.87500000136559564, 1.846868145590734089 ) ) ;
#2478 = CARTESIAN_POINT ( 'NONE',  ( -16.18981371719799611, -5.000000000000000000, -15.95842007673748952 ) ) ;
#2479 = VERTEX_POINT ( 'NONE', #4929 ) ;
#2480 = CARTESIAN_POINT ( 'NONE',  ( 40.98096197216263903, -3.000000000000000000, 26.98110827883376928 ) ) ;
#2481 = CARTESIAN_POINT ( 'NONE',  ( 4.769696007084728073, -20.00000000000000000, 1.500000000000000000 ) ) ;
#2482 = VECTOR ( 'NONE', #4565, 1000.000000000000000 ) ;
#2483 = DIRECTION ( 'NONE',  ( -0.8660254037844377084, -0.5000000000000015543, 0.000000000000000000 ) ) ;
#2484 = DIRECTION ( 'NONE',  ( 0.000000000000000000, 0.000000000000000000, 1.000000000000000000 ) ) ;
#2485 = CARTESIAN_POINT ( 'NONE',  ( -116.3391301858327296, -120.2076149402627294, -7.500000000000000000 ) ) ;
#2486 = CARTESIAN_POINT ( 'NONE',  ( -4.458734125000001214, -25.12500000136559564, 1.846868145590734089 ) ) ;
#2487 = DIRECTION ( 'NONE',  ( -1.319090325525611458E-16, -1.000000000000000000, 0.000000000000000000 ) ) ;
#2488 = AXIS2_PLACEMENT_3D ( 'NONE', #13593, #12461, #8933 ) ;
#2489 = CARTESIAN_POINT ( 'NONE',  ( 4.391654775818395251, -2.390265326283149694, -0.9999999972688140559 ) ) ;
#2490 = CARTESIAN_POINT ( 'NONE',  ( -3.535533905932737309, -28.75000000273118772, -3.535533905932738197 ) ) ;
#2491 = ADVANCED_FACE ( 'NONE', ( #3709 ), #8656, .T. ) ;
#2492 = CARTESIAN_POINT ( 'NONE',  ( 2.621086668468695979, 7.606368536631366695, -7.634085501268425666 ) ) ;
#2493 = DIRECTION ( 'NONE',  ( 0.000000000000000000, 0.000000000000000000, -1.000000000000000000 ) ) ;
#2494 = EDGE_LOOP ( 'NONE', ( #3249, #2943, #8099, #7599 ) ) ;
#2495 = ORIENTED_EDGE ( 'NONE', *, *, #11437, .T. ) ;
#2496 = CARTESIAN_POINT ( 'NONE',  ( -94.14213562373093680, -30.85786437626905965, 17.50000000000000000 ) ) ;
#2497 = VERTEX_POINT ( 'NONE', #88 ) ;
#2498 = CARTESIAN_POINT ( 'NONE',  ( 2.500000000000000000, 0.000000000000000000, 0.000000000000000000 ) ) ;
#2499 = CIRCLE ( 'NONE', #15695, 2.649999999999992806 ) ;
#2500 = EDGE_CURVE ( 'NONE', #6278, #8001, #10693, .T. ) ;
#2501 = CARTESIAN_POINT ( 'NONE',  ( 35.00000000000000000, 37.00000000000000000, -8.572527594031472993E-15 ) ) ;
#2502 = AXIS2_PLACEMENT_3D ( 'NONE', #8052, #3348, #14421 ) ;
#2503 = CARTESIAN_POINT ( 'NONE',  ( -4.276409079477644148, -1.261996585732578335, -3.812499998634404808 ) ) ;
#2504 = APPLICATION_PROTOCOL_DEFINITION ( 'draft international standard', 'automotive_design', 1998, #15891 ) ;
#2505 =( BOUNDED_CURVE ( )  B_SPLINE_CURVE ( 2, ( #2985, #9145, #12992, #4199, #15526, #657, #12916, #1850, #14058, #9224, #5582 ),
 .UNSPECIFIED., .F., .F. ) 
 B_SPLINE_CURVE_WITH_KNOTS ( ( 3, 2, 2, 2, 2, 3 ),
 ( 0.8545872658012773071, 0.8625000000000000444, 0.8750000000000000000, 0.8874999999999999556, 0.9000000000000000222, 0.9045872658012773515 ),
 .UNSPECIFIED. ) 
 CURVE ( )  GEOMETRIC_REPRESENTATION_ITEM ( )  RATIONAL_B_SPLINE_CURVE ( ( 0.9646335149384808183, 0.9518143178943441196, 1.000000000000000000, 0.9238795325112867385, 1.000000000000000000, 0.9238795325112867385, 1.000000000000000000, 0.9238795325112867385, 1.000000000000000000, 0.9720652146169423968, 0.9646335149384803742 ) ) 
 REPRESENTATION_ITEM ( '' )  );
#2506 = CARTESIAN_POINT ( 'NONE',  ( 3.753672977998667726, 3.033343224707664376, -5.499999998634407916 ) ) ;
#2507 = DIRECTION ( 'NONE',  ( 0.000000000000000000, 0.000000000000000000, 1.000000000000000000 ) ) ;
#2508 = CONICAL_SURFACE ( 'NONE', #8226, 2.055000000000000160, 0.7853981633974721488 ) ;
#2509 = CARTESIAN_POINT ( 'NONE',  ( 4.276409079477644148, 1.261996585732577891, -8.437499998634409692 ) ) ;
#2510 = VERTEX_POINT ( 'NONE', #8740 ) ;
#2511 = CARTESIAN_POINT ( 'NONE',  ( 4.830276029870151255, -4.472255266397859863, -48.49891554519376058 ) ) ;
#2512 =( LENGTH_UNIT ( ) NAMED_UNIT ( * ) SI_UNIT ( .MILLI., .METRE. ) );
#2513 = VERTEX_POINT ( 'NONE', #13646 ) ;
#2514 = CARTESIAN_POINT ( 'NONE',  ( 4.197478902586992966, -0.8524102783748346290, -3.505063281295504041 ) ) ;
#2515 = ORIENTED_EDGE ( 'NONE', *, *, #8358, .T. ) ;
#2516 = CIRCLE ( 'NONE', #8745, 5.000000000000000000 ) ;
#2517 = VERTEX_POINT ( 'NONE', #2575 ) ;
#2518 = CARTESIAN_POINT ( 'NONE',  ( -3.033343224707664820, 3.753672977998667726, -3.249999998634409692 ) ) ;
#2519 = CARTESIAN_POINT ( 'NONE',  ( 45.58845726811992449, 0.000000000000000000, -42.96152422706630603 ) ) ;
#2520 = ADVANCED_FACE ( 'NONE', ( #1362 ), #15037, .T. ) ;
#2521 = AXIS2_PLACEMENT_3D ( 'NONE', #7583, #12483, #1423 ) ;
#2522 = ADVANCED_FACE ( 'NONE', ( #8896 ), #2898, .F. ) ;
#2523 =( GEOMETRIC_REPRESENTATION_CONTEXT ( 3 ) GLOBAL_UNCERTAINTY_ASSIGNED_CONTEXT ( ( #479 ) ) GLOBAL_UNIT_ASSIGNED_CONTEXT ( ( #11657, #14256, #6825 ) ) REPRESENTATION_CONTEXT ( 'NONE', 'WORKASPACE' ) );
#2524 = CARTESIAN_POINT ( 'NONE',  ( 3.753672977998667726, 3.033343224707664820, -8.249999998634409692 ) ) ;
#2525 = PLANE ( 'NONE',  #11792 ) ;
#2526 = VECTOR ( 'NONE', #10801, 1000.000000000000000 ) ;
#2527 = UNCERTAINTY_MEASURE_WITH_UNIT (LENGTH_MEASURE( 1.000000000000000082E-05 ), #14882, 'distance_accuracy_value', 'NONE');
#2528 = DIRECTION ( 'NONE',  ( -1.982541115402065110E-16, 1.000000000000000000, 0.000000000000000000 ) ) ;
#2529 = AXIS2_PLACEMENT_3D ( 'NONE', #4066, #2850, #1566 ) ;
#2530 = CARTESIAN_POINT ( 'NONE',  ( -5.381735091635034607, 0.5711823568785950878, -2.437499997268816276 ) ) ;
#2531 = DIRECTION ( 'NONE',  ( 0.000000000000000000, 1.000000000000000000, 0.000000000000000000 ) ) ;
#2532 = CARTESIAN_POINT ( 'NONE',  ( 4.769696007084728073, -20.00000000000000000, -1.500000000000000000 ) ) ;
#2533 = CARTESIAN_POINT ( 'NONE',  ( -8.190561711645485556E-16, -26.93750000136559564, 4.458734124999999437 ) ) ;
#2534 = ORIENTED_EDGE ( 'NONE', *, *, #8630, .F. ) ;
#2535 = DIRECTION ( 'NONE',  ( 0.000000000000000000, 0.000000000000000000, -1.000000000000000000 ) ) ;
#2536 = CARTESIAN_POINT ( 'NONE',  ( 0.5093500532425063732, 4.799145180956616130, -4.124999998634405252 ) ) ;
#2537 = CARTESIAN_POINT ( 'NONE',  ( -35.00000000000000000, 50.00000000000000000, -2.649999999999992806 ) ) ;
#2538 = ORIENTED_EDGE ( 'NONE', *, *, #14897, .F. ) ;
#2539 = VECTOR ( 'NONE', #13072, 1000.000000000000000 ) ;
#2540 = ORIENTED_EDGE ( 'NONE', *, *, #9564, .F. ) ;
#2541 = VECTOR ( 'NONE', #14062, 1000.000000000000000 ) ;
#2542 = DIRECTION ( 'NONE',  ( 1.000000000000000000, 0.000000000000000000, 0.000000000000000000 ) ) ;
#2543 = VERTEX_POINT ( 'NONE', #14051 ) ;
#2544 = CARTESIAN_POINT ( 'NONE',  ( -3.152801135295367985, -23.06250000136559564, 3.152801135295367096 ) ) ;
#2545 = CARTESIAN_POINT ( 'NONE',  ( 0.2500000000000002220, 0.000000000000000000, 4.250000000000000000 ) ) ;
#2546 = DIRECTION ( 'NONE',  ( -0.000000000000000000, -1.000000000000000000, -0.000000000000000000 ) ) ;
#2547 = EDGE_CURVE ( 'NONE', #13637, #6536, #8775, .T. ) ;
#2548 = EDGE_CURVE ( 'NONE', #678, #14655, #1607, .T. ) ;
#2549 = CARTESIAN_POINT ( 'NONE',  ( -34.99999999999999289, -11.00000000000000178, -1.999999999999170441 ) ) ;
#2550 = FACE_BOUND ( 'NONE', #13651, .T. ) ;
#2551 = CARTESIAN_POINT ( 'NONE',  ( 0.000000000000000000, -20.00000000000000000, 5.000000000000000000 ) ) ;
#2552 = VECTOR ( 'NONE', #2922, 999.9999999999998863 ) ;
#2553 = CARTESIAN_POINT ( 'NONE',  ( 5.381735091635035495, -0.5711823568785978633, -1.062500000000000222 ) ) ;
#2554 = CARTESIAN_POINT ( 'NONE',  ( -41.99999999999978684, -11.00000000000000178, -3.500000000000001776 ) ) ;
#2555 = CARTESIAN_POINT ( 'NONE',  ( -114.9999999999999716, -10.00000000000000888, -17.50000000000000000 ) ) ;
#2556 = CARTESIAN_POINT ( 'NONE',  ( 4.458734124999999437, -27.50000000136559208, 1.846868145590737864 ) ) ;
#2557 = CARTESIAN_POINT ( 'NONE',  ( -0.5093500532425060401, -4.799145180956616130, -3.874999998634408360 ) ) ;
#2558 = ORIENTED_EDGE ( 'NONE', *, *, #4185, .T. ) ;
#2559 = PLANE ( 'NONE',  #3238 ) ;
#2560 = ORIENTED_EDGE ( 'NONE', *, *, #5738, .F. ) ;
#2561 = EDGE_LOOP ( 'NONE', ( #1299, #2455, #1699, #1152 ) ) ;
#2562 = DIRECTION ( 'NONE',  ( 0.000000000000000000, 0.000000000000000000, 1.000000000000000000 ) ) ;
#2563 = CARTESIAN_POINT ( 'NONE',  ( 3.152801135295367541, -25.31250000136559564, -3.152801135295367541 ) ) ;
#2564 = DIRECTION ( 'NONE',  ( 1.000000000000000000, 0.000000000000000000, 0.000000000000000000 ) ) ;
#2565 = ORIENTED_EDGE ( 'NONE', *, *, #13620, .T. ) ;
#2566 = CIRCLE ( 'NONE', #8025, 2.499999999999998668 ) ;
#2567 = DIRECTION ( 'NONE',  ( -0.000000000000000000, -0.000000000000000000, -1.000000000000000000 ) ) ;
#2568 = ADVANCED_FACE ( 'NONE', ( #1447 ), #9219, .T. ) ;
#2569 = EDGE_CURVE ( 'NONE', #3401, #4698, #7429, .T. ) ;
#2570 = EDGE_CURVE ( 'NONE', #4563, #14394, #14155, .T. ) ;
#2571 = DIRECTION ( 'NONE',  ( -0.000000000000000000, -1.000000000000000000, -0.000000000000000000 ) ) ;
#2572 = CARTESIAN_POINT ( 'NONE',  ( 3.753672977998667726, 3.033343224707664820, -1.249999998634407916 ) ) ;
#2573 = DIRECTION ( 'NONE',  ( 0.000000000000000000, 0.000000000000000000, -1.000000000000000000 ) ) ;
#2574 = CARTESIAN_POINT ( 'NONE',  ( -2.071067811865475061, -30.68750000000000355, -5.000000000000000888 ) ) ;
#2575 = CARTESIAN_POINT ( 'NONE',  ( 5.000000000000004441, -2.247904837838113790E-16, -3.920263044861760360 ) ) ;
#2576 = CARTESIAN_POINT ( 'NONE',  ( 0.000000000000000000, 0.000000000000000000, 0.000000000000000000 ) ) ;
#2577 = CARTESIAN_POINT ( 'NONE',  ( -5.000000000000000000, -26.62500000273118772, -6.123233995736766282E-16 ) ) ;
#2578 = LINE ( 'NONE', #14966, #353 ) ;
#2579 = CARTESIAN_POINT ( 'NONE',  ( 3.152801135295366208, -29.56250000136559208, 3.152801135295367985 ) ) ;
#2580 = DIRECTION ( 'NONE',  ( 1.000000000000000000, 0.000000000000000000, 0.000000000000000000 ) ) ;
#2581 = ORIENTED_EDGE ( 'NONE', *, *, #1261, .T. ) ;
#2582 = ORIENTED_EDGE ( 'NONE', *, *, #10966, .T. ) ;
#2583 = SURFACE_SIDE_STYLE ('',( #8003 ) ) ;
#2584 = ORIENTED_EDGE ( 'NONE', *, *, #13761, .T. ) ;
#2585 = DIRECTION ( 'NONE',  ( 0.000000000000000000, 0.000000000000000000, -1.000000000000000000 ) ) ;
#2586 = ORIENTED_EDGE ( 'NONE', *, *, #1126, .F. ) ;
#2587 = FACE_OUTER_BOUND ( 'NONE', #9380, .T. ) ;
#2588 = B_SPLINE_CURVE_WITH_KNOTS ( 'NONE', 3,
 ( #10155, #6448, #9187, #8948, #6596 ),
 .UNSPECIFIED., .F., .F.,
 ( 4, 1, 4 ),
 ( 0.000000000000000000, 0.002309401076758505356, 0.004618802153517010713 ),
 .UNSPECIFIED. ) ;
#2589 = EDGE_CURVE ( 'NONE', #14039, #7722, #9908, .T. ) ;
#2590 = CARTESIAN_POINT ( 'NONE',  ( -4.795541693661363958, -1.415196051561583790, -4.374999997268816720 ) ) ;
#2591 = CARTESIAN_POINT ( 'NONE',  ( 3.033343224707661712, -3.753672977998669946, -4.499999998634407028 ) ) ;
#2592 = PRODUCT_CONTEXT ( 'NONE', #12774, 'mechanical' ) ;
#2593 = CARTESIAN_POINT ( 'NONE',  ( 3.916244202832140253, -2.131511515620588160, -6.687499998634407028 ) ) ;
#2594 = DIRECTION ( 'NONE',  ( 1.000000000000000000, 0.000000000000000000, -0.000000000000000000 ) ) ;
#2595 = CARTESIAN_POINT ( 'NONE',  ( 2.071067811865461294, -23.81250000000000000, -5.000000000000014211 ) ) ;
#2596 = EDGE_LOOP ( 'NONE', ( #9917, #6295, #11447, #4939 ) ) ;
#2597 = CARTESIAN_POINT ( 'NONE',  ( -7.500000000000003553, 1.443375672974063662, -7.063244554130003294 ) ) ;
#2598 =( NAMED_UNIT ( * ) SI_UNIT ( $, .STERADIAN. ) SOLID_ANGLE_UNIT ( ) );
#2599 = EDGE_CURVE ( 'NONE', #7177, #15428, #8011, .T. ) ;
#2600 = EDGE_LOOP ( 'NONE', ( #15728, #10436, #7534, #8946 ) ) ;
#2601 = LINE ( 'NONE', #7553, #12108 ) ;
#2602 = DIRECTION ( 'NONE',  ( 0.000000000000000000, 0.000000000000000000, 1.000000000000000000 ) ) ;
#2603 = ORIENTED_EDGE ( 'NONE', *, *, #3126, .F. ) ;
#2604 = ITEM_DEFINED_TRANSFORMATION ( 'NONE', 'NONE', #6842,  #3223 ) ;
#2605 = CARTESIAN_POINT ( 'NONE',  ( -2.131511515620587272, -3.916244202832140253, -5.937499998634407028 ) ) ;
#2606 = LINE ( 'NONE', #365, #4522 ) ;
#2607 = PRODUCT_DEFINITION_SHAPE ( 'NONE', 'NONE',  #15997 ) ;
#2608 =( BOUNDED_CURVE ( )  B_SPLINE_CURVE ( 2, ( #14735, #9566, #5850, #2120, #14656, #13258, #9635, #14494, #13490 ),
 .UNSPECIFIED., .F., .F. ) 
 B_SPLINE_CURVE_WITH_KNOTS ( ( 3, 2, 2, 2, 3 ),
 ( 0.9250000000000002665, 0.9375000000000002220, 0.9500000000000001776, 0.9625000000000002442, 0.9750000000000001998 ),
 .UNSPECIFIED. ) 
 CURVE ( )  GEOMETRIC_REPRESENTATION_ITEM ( )  RATIONAL_B_SPLINE_CURVE ( ( 0.9999999999999986677, 0.9238795325112880708, 1.000000000000000000, 0.9238795325112867385, 1.000000000000000000, 0.9238795325112867385, 1.000000000000000000, 0.9238795325112854062, 1.000000000000001332 ) ) 
 REPRESENTATION_ITEM ( '' )  );
#2609 = CARTESIAN_POINT ( 'NONE',  ( 2.500000000000000000, -1.768423874527823569, 1.021000000000002794 ) ) ;
#2610 = PLANE ( 'NONE',  #11285 ) ;
#2611 = DIRECTION ( 'NONE',  ( -0.000000000000000000, 1.000000000000000000, -0.000000000000000000 ) ) ;
#2612 = CARTESIAN_POINT ( 'NONE',  ( 3.401574460001763001, -4.209348295687703967, -5.062499997268816720 ) ) ;
#2613 = DIRECTION ( 'NONE',  ( 0.9999824063907751803, 0.005931855436079011210, -0.000000000000000000 ) ) ;
#2614 = CARTESIAN_POINT ( 'NONE',  ( 4.458734124999999437, -31.68750000136559564, 0.000000000000000000 ) ) ;
#2615 = CARTESIAN_POINT ( 'NONE',  ( 1.846868145590735200, -25.50000000136559919, -4.458734124999999437 ) ) ;
#2616 = VERTEX_POINT ( 'NONE', #12746 ) ;
#2617 = DIRECTION ( 'NONE',  ( 0.000000000000000000, 0.000000000000000000, -1.000000000000000000 ) ) ;
#2618 = CARTESIAN_POINT ( 'NONE',  ( -0.5093500532425060401, -4.799145180956616130, -6.624999998634407916 ) ) ;
#2619 = CARTESIAN_POINT ( 'NONE',  ( -21.01110699893041911, -3.000000000000001332, -33.74230484541335784 ) ) ;
#2620 = EDGE_CURVE ( 'NONE', #11629, #6271, #8818, .T. ) ;
#2621 = VERTEX_POINT ( 'NONE', #14297 ) ;
#2622 = ORIENTED_EDGE ( 'NONE', *, *, #14803, .T. ) ;
#2623 = AXIS2_PLACEMENT_3D ( 'NONE', #11080, #6153, #13469 ) ;
#2624 = EDGE_CURVE ( 'NONE', #7223, #8388, #4671, .T. ) ;
#2625 = FILL_AREA_STYLE_COLOUR ( '', #6323 ) ;
#2626 = VERTEX_POINT ( 'NONE', #5726 ) ;
#2627 = CARTESIAN_POINT ( 'NONE',  ( -1.846868145590737420, -22.00000000136559208, 4.458734124999999437 ) ) ;
#2628 = CARTESIAN_POINT ( 'NONE',  ( -5.725490332117410652, -3.000000000000000000, 49.91684015347181003 ) ) ;
#2629 = LINE ( 'NONE', #8869, #12226 ) ;
#2630 = CARTESIAN_POINT ( 'NONE',  ( -44.99999999999999289, -11.00000000000000178, -3.999999999999170885 ) ) ;
#2631 = CARTESIAN_POINT ( 'NONE',  ( -2.621328321947914208, -7.606199919102974327, -7.633618187056795179 ) ) ;
#2632 = DIRECTION ( 'NONE',  ( 1.982541115402065110E-16, -1.000000000000000000, -0.000000000000000000 ) ) ;
#2633 = CARTESIAN_POINT ( 'NONE',  ( -5.381735091635034607, 0.5711823568785950878, -3.562499999999998224 ) ) ;
#2634 = CARTESIAN_POINT ( 'NONE',  ( 2.071067811865497710, -30.18750000000000355, 4.999999999999978684 ) ) ;
#2635 = CONICAL_SURFACE ( 'NONE', #14525, 4.000000000000000000, 0.8911886515913786111 ) ;
#2636 = CARTESIAN_POINT ( 'NONE',  ( 3.535533905932738197, -28.87500000000000000, -3.535533905932738197 ) ) ;
#2637 = CARTESIAN_POINT ( 'NONE',  ( -3.152801135295367985, -24.81250000136559564, 3.152801135295367096 ) ) ;
#2638 = CARTESIAN_POINT ( 'NONE',  ( 4.276409079477644148, 1.261996585732577891, -1.562499998634406140 ) ) ;
#2639 = ORIENTED_EDGE ( 'NONE', *, *, #2061, .T. ) ;
#2640 = CARTESIAN_POINT ( 'NONE',  ( 5.200000000000002842, 0.000000000000000000, 2.500000000000000888 ) ) ;
#2641 = ORIENTED_EDGE ( 'NONE', *, *, #9390, .T. ) ;
#2642 = ORIENTED_EDGE ( 'NONE', *, *, #7627, .T. ) ;
#2643 = ADVANCED_FACE ( 'NONE', ( #6871 ), #12910, .F. ) ;
#2644 = PRODUCT_RELATED_PRODUCT_CATEGORY ( 'part', '', ( #9518 ) ) ;
#2645 = CARTESIAN_POINT ( 'NONE',  ( -3.152801135295367985, -25.81250000136559564, 3.152801135295367096 ) ) ;
#2646 = DIRECTION ( 'NONE',  ( 0.000000000000000000, 0.000000000000000000, 1.000000000000000000 ) ) ;
#2647 = ORIENTED_EDGE ( 'NONE', *, *, #3701, .T. ) ;
#2648 = AXIS2_PLACEMENT_3D ( 'NONE', #3792, #5089, #15849 ) ;
#2649 = FACE_OUTER_BOUND ( 'NONE', #11353, .T. ) ;
#2650 = DIRECTION ( 'NONE',  ( 1.000000000000000000, 0.000000000000000000, 0.000000000000000000 ) ) ;
#2651 = DIRECTION ( 'NONE',  ( -1.000000000000000000, 0.000000000000000000, -0.000000000000000000 ) ) ;
#2652 = CARTESIAN_POINT ( 'NONE',  ( 4.458734124999998549, -3.052311964297492742E-11, -0.3789984458506765463 ) ) ;
#2653 = CARTESIAN_POINT ( 'NONE',  ( -5.000000000000000888, -30.43750000000000355, 2.071067811865474617 ) ) ;
#2654 = PLANE ( 'NONE',  #3400 ) ;
#2655 = DIRECTION ( 'NONE',  ( 1.000000000000000000, -4.440892098500626162E-15, 0.000000000000000000 ) ) ;
#2656 = CARTESIAN_POINT ( 'NONE',  ( 2.071067811865475505, -26.93750000273119127, -5.000000000000000888 ) ) ;
#2657 = CARTESIAN_POINT ( 'NONE',  ( 5.000000000000004441, -2.247904837838113790E-16, -3.045263047592945860 ) ) ;
#2658 = CARTESIAN_POINT ( 'NONE',  ( 4.458734124999997661, -30.50000000136559919, 1.846868145590737864 ) ) ;
#2659 = EDGE_CURVE ( 'NONE', #2847, #3269, #15607, .T. ) ;
#2660 = SURFACE_STYLE_FILL_AREA ( #342 ) ;
#2661 = ORIENTED_EDGE ( 'NONE', *, *, #14112, .F. ) ;
#2662 = ORIENTED_EDGE ( 'NONE', *, *, #12701, .F. ) ;
#2663 = ADVANCED_FACE ( 'NONE', ( #14379, #8092 ), #12010, .T. ) ;
#2664 = FILL_AREA_STYLE_COLOUR ( '', #3713 ) ;
#2665 = ORIENTED_EDGE ( 'NONE', *, *, #3366, .T. ) ;
#2666 = CARTESIAN_POINT ( 'NONE',  ( 19.99999999999956657, -8.786575603324269439E-13, 1.500000000000000000 ) ) ;
#2667 = ORIENTED_EDGE ( 'NONE', *, *, #3812, .F. ) ;
#2668 = CARTESIAN_POINT ( 'NONE',  ( 9.184850993605150311E-15, 37.00000000000000000, -75.00000000000001421 ) ) ;
#2669 = CIRCLE ( 'NONE', #11704, 2.700000000000001066 ) ;
#2670 = FACE_OUTER_BOUND ( 'NONE', #12081, .T. ) ;
#2671 = APPLICATION_PROTOCOL_DEFINITION ( 'draft international standard', 'automotive_design', 1998, #1957 ) ;
#2672 = CARTESIAN_POINT ( 'NONE',  ( -4.799145180956616130, 0.5093500532425063732, -7.124999998634407916 ) ) ;
#2673 = DIRECTION ( 'NONE',  ( 0.000000000000000000, 0.000000000000000000, 1.000000000000000000 ) ) ;
#2674 = CARTESIAN_POINT ( 'NONE',  ( 7.500000000000001776, 0.000000000000000000, 0.000000000000000000 ) ) ;
#2675 = EDGE_LOOP ( 'NONE', ( #11553, #9109, #13096, #1257 ) ) ;
#2676 = DIRECTION ( 'NONE',  ( -0.000000000000000000, -1.000000000000000000, -0.000000000000000000 ) ) ;
#2677 = EDGE_CURVE ( 'NONE', #4915, #3061, #10820, .T. ) ;
#2678 = ORIENTED_EDGE ( 'NONE', *, *, #9478, .T. ) ;
#2679 = CARTESIAN_POINT ( 'NONE',  ( 5.200000000000002842, 3.061616997868384127E-16, -2.500000000000000888 ) ) ;
#2680 = LINE ( 'NONE', #15061, #6377 ) ;
#2681 = COLOUR_RGB ( '', 0.72549020, 0.75294118, 0.79215686) ;
#2682 = ORIENTED_EDGE ( 'NONE', *, *, #12641, .T. ) ;
#2683 = ITEM_DEFINED_TRANSFORMATION ( 'NONE', 'NONE', #6573,  #3223 ) ;
#2684 = CARTESIAN_POINT ( 'NONE',  ( -1.261996585732579224, 4.276409079477648589, -5.312499998634406140 ) ) ;
#2685 = CIRCLE ( 'NONE', #8936, 2.649999999999985700 ) ;
#2686 = CIRCLE ( 'NONE', #10444, 2.649999999999985700 ) ;
#2687 = CARTESIAN_POINT ( 'NONE',  ( 5.000000000000002665, 1.275685995473128912E-14, -4.920263044861760804 ) ) ;
#2688 = CARTESIAN_POINT ( 'NONE',  ( 17.00000000000000000, 0.000000000000000000, 0.000000000000000000 ) ) ;
#2689 = DIRECTION ( 'NONE',  ( 0.000000000000000000, 0.000000000000000000, 1.000000000000000000 ) ) ;
#2690 = PRODUCT_DEFINITION_CONTEXT ( 'detailed design', #15187, 'design' ) ;
#2691 = CARTESIAN_POINT ( 'NONE',  ( 1.567478505476134606E-15, 4.618802153517012066, -3.433295621305382905 ) ) ;
#2692 = AXIS2_PLACEMENT_3D ( 'NONE', #11279, #14682, #1171 ) ;
#2693 = CARTESIAN_POINT ( 'NONE',  ( -3.401574460001764777, 4.209348295687701302, -5.562499997268814056 ) ) ;
#2694 = CARTESIAN_POINT ( 'NONE',  ( -3.535533905932737309, -23.62500000000000000, -3.535533905932738197 ) ) ;
#2695 = CARTESIAN_POINT ( 'NONE',  ( 3.535533905932738197, -28.00000000273118772, -3.535533905932738197 ) ) ;
#2696 = DIRECTION ( 'NONE',  ( -0.8660254037844408170, -0.000000000000000000, -0.4999999999999961142 ) ) ;
#2697 = ORIENTED_EDGE ( 'NONE', *, *, #6546, .F. ) ;
#2698 = CARTESIAN_POINT ( 'NONE',  ( 5.200000000000002842, 3.061616997868383634E-16, -2.500000000000000444 ) ) ;
#2699 = B_SPLINE_CURVE_WITH_KNOTS ( 'NONE', 3,
 ( #4885, #8611, #209, #290, #9969, #14910, #10220, #9885 ),
 .UNSPECIFIED., .F., .F.,
 ( 4, 2, 2, 4 ),
 ( 0.005725059856848645212, 0.006314084072593634418, 0.006903108288338624492, 0.008081156719828603771 ),
 .UNSPECIFIED. ) ;
#2700 = CARTESIAN_POINT ( 'NONE',  ( 3.916244202832140253, -2.131511515620588160, -6.437499998634407028 ) ) ;
#2701 = FACE_BOUND ( 'NONE', #2146, .T. ) ;
#2702 = ORIENTED_EDGE ( 'NONE', *, *, #8509, .T. ) ;
#2703 = ORIENTED_EDGE ( 'NONE', *, *, #11988, .F. ) ;
#2704 = ORIENTED_EDGE ( 'NONE', *, *, #13922, .T. ) ;
#2705 = DIRECTION ( 'NONE',  ( 0.000000000000000000, 1.000000000000000000, 0.000000000000000000 ) ) ;
#2706 =( BOUNDED_SURFACE ( )  B_SPLINE_SURFACE ( 1, 2, ( 
 ( #6810, #15300, #8408, #6895, #7196, #13987, #2242, #12097, #14169, #3098, #1036, #11719, #12854, #5971, #10892, #10371, #670, #4135, #11801, #9083, #1794, #6742, #11642, #753, #10446, #15468, #4389, #2919, #6657, #9321, #14244, #10615, #15543, #9840, #8801, #2324, #15835, #15915, #9761, #9914, #14854, #4835, #7268, #153, #13705, #14698, #7342, #4753, #2638, #9674, #12169, #11132, #14945, #12488, #1107, #3532, #6048, #8564, #1428, #71, #13386, #6375, #7510, #13534, #1347, #13452, #14613, #3620, #6133, #8489, #10974, #2393, #7591, #3862, #10004, #12411, #3776, #12249, #1189, #2471, #12334, #11061, #7430, #1201, #6216, #2557, #4914, #6294, #14771, #3693, #8639, #4989, #1271, #8723, #13628, #11209, #5074, #15019, #11606, #12896, #13950, #4177, #1828, #14123, #11372, #1522, #2958, #4098, #9122, #11446, #11526, #7909, #5163, #9202, #2807, #1594, #10337, #5232, #557, #2717, #15263, #11293, #13873, #12653, #7834, #12810, #9047, #10168, #12729, #6459, #1752, #7996, #322, #3934, #1668, #15091, #245, #7762, #10092, #5477, #477, #6703, #6610, #3050, #7675, #8878, #10406, #4011, #13784, #12573, #8963, #392, #5401, #6532, #5313, #10256, #14032, #15342, #4258, #15180, #2881 ),
 ( #10803, #11916, #9582, #15743, #9285, #1990, #4346, #9432, #14360, #10723, #3433, #14206, #941, #4655, #6851, #3130, #4575, #8152, #11991, #14512, #11681, #13136, #5870, #8236, #8387, #13277, #6773, #15425, #3289, #11758, #634, #8314, #9510, #5555, #864, #10492, #8074, #12970, #6939, #1907, #2070, #7014, #15658, #714, #5637, #10580, #15505, #4421, #9356, #14442, #13049, #14281, #3203, #11842, #5785, #791, #3367, #5711, #10646, #15580, #4497, #13203, #2142, #7090, #3842, #14923, #7173, #11188, #6273, #12393, #9896, #1250, #5053, #13366, #10523, #14751, #2307, #4897, #7252, #8621, #4969, #12075, #8702, #12152, #8785, #14676, #7407, #1329, #1089, #6030, #6111, #15816, #5952, #2536, #2219, #9822, #11115, #1019, #9983, #10952, #8467, #14835, #11038, #53, #2376, #2452, #3753, #10872, #133, #9737, #8548, #6198, #15894, #7490, #9653, #13605, #4731, #4815, #3601, #3674, #14588, #13514, #13436, #12311, #7324, #3509, #12228, #1167, #6354, #15159, #2700, #4236, #10149, #2618, #14011, #13933, #15246, #4076, #5458, #5144, #13687, #2936, #8860, #12470, #10388, #7572, #2785, #7815, #5214, #1409, #12554, #10234, #5378, #12709, #15073, #7743, #12634, #6590, #11273, #541, #13766 ) ),
 .UNSPECIFIED., .F., .F., .F. ) 
 B_SPLINE_SURFACE_WITH_KNOTS ( ( 2, 2 ),
 ( 3, 2, 2, 2, 2, 2, 2, 2, 2, 2, 2, 2, 2, 2, 2, 2, 2, 2, 2, 2, 2, 2, 2, 2, 2, 2, 2, 2, 2, 2, 2, 2, 2, 2, 2, 2, 2, 2, 2, 2, 2, 2, 2, 2, 2, 2, 2, 2, 2, 2, 2, 2, 2, 2, 2, 2, 2, 2, 2, 2, 2, 2, 2, 2, 2, 2, 2, 2, 2, 2, 2, 2, 2, 2, 2, 2, 2, 2, 2, 2, 3 ),
 ( 0.000000000000000000, 1.000000000000000000 ),
 ( 0.000000000000000000, 0.01250000000000000069, 0.02500000000000000139, 0.03749999999999999861, 0.05000000000000000278, 0.06250000000000000000, 0.07499999999999999722, 0.08749999999999999445, 0.1000000000000000056, 0.1125000000000000028, 0.1250000000000000000, 0.1375000000000000111, 0.1499999999999999944, 0.1625000000000000056, 0.1749999999999999889, 0.1875000000000000000, 0.2000000000000000111, 0.2124999999999999944, 0.2250000000000000056, 0.2374999999999999889, 0.2500000000000000000, 0.2625000000000000111, 0.2750000000000000222, 0.2874999999999999778, 0.2999999999999999889, 0.3125000000000000000, 0.3250000000000000111, 0.3375000000000000222, 0.3499999999999999778, 0.3624999999999999889, 0.3750000000000000000, 0.3875000000000000111, 0.4000000000000000222, 0.4124999999999999778, 0.4249999999999999889, 0.4375000000000000000, 0.4500000000000000111, 0.4625000000000000222, 0.4749999999999999778, 0.4874999999999999889, 0.5000000000000000000, 0.5124999999999999556, 0.5250000000000000222, 0.5374999999999999778, 0.5500000000000000444, 0.5625000000000000000, 0.5749999999999999556, 0.5875000000000000222, 0.5999999999999999778, 0.6125000000000000444, 0.6250000000000000000, 0.6374999999999999556, 0.6500000000000000222, 0.6624999999999999778, 0.6750000000000000444, 0.6875000000000000000, 0.6999999999999999556, 0.7125000000000000222, 0.7249999999999999778, 0.7375000000000000444, 0.7500000000000000000, 0.7624999999999999556, 0.7750000000000000222, 0.7874999999999999778, 0.8000000000000000444, 0.8125000000000000000, 0.8249999999999999556, 0.8375000000000000222, 0.8499999999999999778, 0.8625000000000000444, 0.8750000000000000000, 0.8874999999999999556, 0.9000000000000000222, 0.9124999999999999778, 0.9250000000000000444, 0.9375000000000000000, 0.9499999999999999556, 0.9625000000000000222, 0.9749999999999999778, 0.9875000000000000444, 1.000000000000000000 ),
 .UNSPECIFIED. ) 
 GEOMETRIC_REPRESENTATION_ITEM ( )  RATIONAL_B_SPLINE_SURFACE ( (
 ( 1.000000000000000000, 0.9238795325112867385, 1.000000000000000000, 0.9238795325112867385, 1.000000000000000000, 0.9238795325112867385, 1.000000000000000000, 0.9238795325112867385, 1.000000000000000000, 0.9238795325112867385, 1.000000000000000000, 0.9238795325112867385, 1.000000000000000000, 0.9238795325112867385, 1.000000000000000000, 0.9238795325112867385, 1.000000000000000000, 0.9238795325112867385, 1.000000000000000000, 0.9238795325112867385, 1.000000000000000000, 0.9238795325112867385, 1.000000000000000000, 0.9238795325112867385, 1.000000000000000000, 0.9238795325112867385, 1.000000000000000000, 0.9238795325112867385, 1.000000000000000000, 0.9238795325112867385, 1.000000000000000000, 0.9238795325112867385, 1.000000000000000000, 0.9238795325112867385, 1.000000000000000000, 0.9238795325112867385, 1.000000000000000000, 0.9238795325112867385, 1.000000000000000000, 0.9238795325112867385, 1.000000000000000000, 0.9238795325112867385, 1.000000000000000000, 0.9238795325112867385, 1.000000000000000000, 0.9238795325112867385, 1.000000000000000000, 0.9238795325112867385, 1.000000000000000000, 0.9238795325112867385, 1.000000000000000000, 0.9238795325112867385, 1.000000000000000000, 0.9238795325112867385, 1.000000000000000000, 0.9238795325112867385, 1.000000000000000000, 0.9238795325112867385, 1.000000000000000000, 0.9238795325112867385, 1.000000000000000000, 0.9238795325112867385, 1.000000000000000000, 0.9238795325112867385, 1.000000000000000000, 0.9238795325112867385, 1.000000000000000000, 0.9238795325112867385, 1.000000000000000000, 0.9238795325112867385, 1.000000000000000000, 0.9238795325112867385, 1.000000000000000000, 0.9238795325112867385, 1.000000000000000000, 0.9238795325112867385, 1.000000000000000000, 0.9238795325112867385, 1.000000000000000000, 0.9238795325112867385, 1.000000000000000000, 0.9238795325112867385, 1.000000000000000000, 0.9238795325112867385, 1.000000000000000000, 0.9238795325112867385, 1.000000000000000000, 0.9238795325112867385, 1.000000000000000000, 0.9238795325112867385, 1.000000000000000000, 0.9238795325112867385, 1.000000000000000000, 0.9238795325112867385, 1.000000000000000000, 0.9238795325112867385, 1.000000000000000000, 0.9238795325112867385, 1.000000000000000000, 0.9238795325112867385, 1.000000000000000000, 0.9238795325112867385, 1.000000000000000000, 0.9238795325112867385, 1.000000000000000000, 0.9238795325112867385, 1.000000000000000000, 0.9238795325112867385, 1.000000000000000000, 0.9238795325112867385, 1.000000000000000000, 0.9238795325112867385, 1.000000000000000000, 0.9238795325112867385, 1.000000000000000000, 0.9238795325112867385, 1.000000000000000000, 0.9238795325112867385, 1.000000000000000000, 0.9238795325112867385, 1.000000000000000000, 0.9238795325112867385, 1.000000000000000000, 0.9238795325112867385, 1.000000000000000000, 0.9238795325112867385, 1.000000000000000000, 0.9238795325112867385, 1.000000000000000000, 0.9238795325112867385, 1.000000000000000000, 0.9238795325112867385, 1.000000000000000000, 0.9238795325112867385, 1.000000000000000000, 0.9238795325112867385, 1.000000000000000000, 0.9238795325112867385, 1.000000000000000000, 0.9238795325112867385, 1.000000000000000000, 0.9238795325112867385, 1.000000000000000000, 0.9238795325112867385, 1.000000000000000000, 0.9238795325112867385, 1.000000000000000000, 0.9238795325112867385, 1.000000000000000000, 0.9238795325112867385, 1.000000000000000000, 0.9238795325112867385, 1.000000000000000000, 0.9238795325112867385, 1.000000000000000000, 0.9238795325112867385, 1.000000000000000000, 0.9238795325112867385, 1.000000000000000000, 0.9238795325112867385, 1.000000000000000000),
 ( 1.000000000000000000, 0.9238795325112867385, 1.000000000000000000, 0.9238795325112867385, 1.000000000000000000, 0.9238795325112867385, 1.000000000000000000, 0.9238795325112867385, 1.000000000000000000, 0.9238795325112867385, 1.000000000000000000, 0.9238795325112867385, 1.000000000000000000, 0.9238795325112867385, 1.000000000000000000, 0.9238795325112867385, 1.000000000000000000, 0.9238795325112867385, 1.000000000000000000, 0.9238795325112867385, 1.000000000000000000, 0.9238795325112867385, 1.000000000000000000, 0.9238795325112867385, 1.000000000000000000, 0.9238795325112867385, 1.000000000000000000, 0.9238795325112867385, 1.000000000000000000, 0.9238795325112867385, 1.000000000000000000, 0.9238795325112867385, 1.000000000000000000, 0.9238795325112867385, 1.000000000000000000, 0.9238795325112867385, 1.000000000000000000, 0.9238795325112867385, 1.000000000000000000, 0.9238795325112867385, 1.000000000000000000, 0.9238795325112867385, 1.000000000000000000, 0.9238795325112867385, 1.000000000000000000, 0.9238795325112867385, 1.000000000000000000, 0.9238795325112867385, 1.000000000000000000, 0.9238795325112867385, 1.000000000000000000, 0.9238795325112867385, 1.000000000000000000, 0.9238795325112867385, 1.000000000000000000, 0.9238795325112867385, 1.000000000000000000, 0.9238795325112867385, 1.000000000000000000, 0.9238795325112867385, 1.000000000000000000, 0.9238795325112867385, 1.000000000000000000, 0.9238795325112867385, 1.000000000000000000, 0.9238795325112867385, 1.000000000000000000, 0.9238795325112867385, 1.000000000000000000, 0.9238795325112867385, 1.000000000000000000, 0.9238795325112867385, 1.000000000000000000, 0.9238795325112867385, 1.000000000000000000, 0.9238795325112867385, 1.000000000000000000, 0.9238795325112867385, 1.000000000000000000, 0.9238795325112867385, 1.000000000000000000, 0.9238795325112867385, 1.000000000000000000, 0.9238795325112867385, 1.000000000000000000, 0.9238795325112867385, 1.000000000000000000, 0.9238795325112867385, 1.000000000000000000, 0.9238795325112867385, 1.000000000000000000, 0.9238795325112867385, 1.000000000000000000, 0.9238795325112867385, 1.000000000000000000, 0.9238795325112867385, 1.000000000000000000, 0.9238795325112867385, 1.000000000000000000, 0.9238795325112867385, 1.000000000000000000, 0.9238795325112867385, 1.000000000000000000, 0.9238795325112867385, 1.000000000000000000, 0.9238795325112867385, 1.000000000000000000, 0.9238795325112867385, 1.000000000000000000, 0.9238795325112867385, 1.000000000000000000, 0.9238795325112867385, 1.000000000000000000, 0.9238795325112867385, 1.000000000000000000, 0.9238795325112867385, 1.000000000000000000, 0.9238795325112867385, 1.000000000000000000, 0.9238795325112867385, 1.000000000000000000, 0.9238795325112867385, 1.000000000000000000, 0.9238795325112867385, 1.000000000000000000, 0.9238795325112867385, 1.000000000000000000, 0.9238795325112867385, 1.000000000000000000, 0.9238795325112867385, 1.000000000000000000, 0.9238795325112867385, 1.000000000000000000, 0.9238795325112867385, 1.000000000000000000, 0.9238795325112867385, 1.000000000000000000, 0.9238795325112867385, 1.000000000000000000, 0.9238795325112867385, 1.000000000000000000, 0.9238795325112867385, 1.000000000000000000, 0.9238795325112867385, 1.000000000000000000, 0.9238795325112867385, 1.000000000000000000, 0.9238795325112867385, 1.000000000000000000, 0.9238795325112867385, 1.000000000000000000, 0.9238795325112867385, 1.000000000000000000, 0.9238795325112867385, 1.000000000000000000, 0.9238795325112867385, 1.000000000000000000, 0.9238795325112867385, 1.000000000000000000, 0.9238795325112867385, 1.000000000000000000) ) ) 
 REPRESENTATION_ITEM ( '' )  SURFACE ( )  );
#2707 = COLOUR_RGB ( '', 0.72549020, 0.75294118, 0.79215686) ;
#2708 = LINE ( 'NONE', #234, #13017 ) ;
#2709 = EDGE_CURVE ( 'NONE', #10113, #15266, #15594, .T. ) ;
#2710 = DIRECTION ( 'NONE',  ( 0.000000000000000000, 0.000000000000000000, 1.000000000000000000 ) ) ;
#2711 = CARTESIAN_POINT ( 'NONE',  ( 0.04725809328185395092, -9.175759667312529899, -8.057670357645365655 ) ) ;
#2712 = LINE ( 'NONE', #12405, #12601 ) ;
#2713 = CARTESIAN_POINT ( 'NONE',  ( 4.209348295687701302, 3.401574460001765665, -6.937500000000004441 ) ) ;
#2714 = DIRECTION ( 'NONE',  ( -1.000000000000000000, -1.239088197126290324E-16, 0.000000000000000000 ) ) ;
#2715 = CARTESIAN_POINT ( 'NONE',  ( -4.140404888673278272, -2.228338276487456415, -3.686887068327035166 ) ) ;
#2716 = CARTESIAN_POINT ( 'NONE',  ( 4.458734124999999437, -23.50000000136559564, 1.846868145590737864 ) ) ;
#2717 = CARTESIAN_POINT ( 'NONE',  ( -3.753672977998669946, -3.033343224707661712, -5.999999998634407916 ) ) ;
#2718 = ORIENTED_EDGE ( 'NONE', *, *, #5141, .F. ) ;
#2719 = AXIS2_PLACEMENT_3D ( 'NONE', #15918, #11211, #9916 ) ;
#2720 = CARTESIAN_POINT ( 'NONE',  ( -60.00000000000000000, -4.999999999999997335, -20.00000000000000711 ) ) ;
#2721 = ORIENTED_EDGE ( 'NONE', *, *, #7757, .T. ) ;
#2722 = ORIENTED_EDGE ( 'NONE', *, *, #14976, .T. ) ;
#2723 = AXIS2_PLACEMENT_3D ( 'NONE', #1059, #15942, #2585 ) ;
#2724 = AXIS2_PLACEMENT_3D ( 'NONE', #8341, #13233, #10676 ) ;
#2725 = CARTESIAN_POINT ( 'NONE',  ( 2.730187237215162345E-16, -22.18750000136559564, -4.458734124999999437 ) ) ;
#2726 = DIRECTION ( 'NONE',  ( 0.000000000000000000, 1.000000000000000000, 0.000000000000000000 ) ) ;
#2727 = ORIENTED_EDGE ( 'NONE', *, *, #13000, .F. ) ;
#2728 = CARTESIAN_POINT ( 'NONE',  ( -17.99999999999979394, -9.000000000000001776, 1.499999999999999112 ) ) ;
#2729 = AXIS2_PLACEMENT_3D ( 'NONE', #4100, #8077, #481 ) ;
#2730 = DIRECTION ( 'NONE',  ( -1.000000000000000000, 0.000000000000000000, 0.000000000000000000 ) ) ;
#2731 = EDGE_CURVE ( 'NONE', #15878, #1169, #11203, .T. ) ;
#2732 = CARTESIAN_POINT ( 'NONE',  ( 4.313165601266488736, -1.402244460665938997, -0.4094021847041934281 ) ) ;
#2733 = DIRECTION ( 'NONE',  ( 0.000000000000000000, 0.000000000000000000, 1.000000000000000000 ) ) ;
#2734 = EDGE_CURVE ( 'NONE', #615, #7914, #2686, .T. ) ;
#2735 = CIRCLE ( 'NONE', #5835, 10.00000000000000533 ) ;
#2736 = CARTESIAN_POINT ( 'NONE',  ( 2.071067811865476394, -28.18750000000000711, 5.000000000000000000 ) ) ;
#2737 = CARTESIAN_POINT ( 'NONE',  ( -44.29779928441806902, -3.660959011663034612, -20.50864992044095558 ) ) ;
#2738 = DIRECTION ( 'NONE',  ( -0.000000000000000000, 1.000000000000000000, -0.000000000000000000 ) ) ;
#2739 = CARTESIAN_POINT ( 'NONE',  ( -5.000000000000000888, -27.68750000273119127, -2.071067811865475949 ) ) ;
#2740 = DIRECTION ( 'NONE',  ( 0.8660254037844410391, 0.4999999999999958367, -0.000000000000000000 ) ) ;
#2741 = CARTESIAN_POINT ( 'NONE',  ( -8.190561711645485556E-16, -29.68750000136559208, 4.458734124999999437 ) ) ;
#2742 = CARTESIAN_POINT ( 'NONE',  ( -1.154700538379255903, -35.00000000000000000, 34.00000000000000711 ) ) ;
#2743 = EDGE_LOOP ( 'NONE', ( #11065, #6512 ) ) ;
#2744 = AXIS2_PLACEMENT_3D ( 'NONE', #6916, #10558, #12951 ) ;
#2745 = ORIENTED_EDGE ( 'NONE', *, *, #6491, .T. ) ;
#2746 = FILL_AREA_STYLE_COLOUR ( '', #6315 ) ;
#2747 = ORIENTED_EDGE ( 'NONE', *, *, #316, .T. ) ;
#2748 = CARTESIAN_POINT ( 'NONE',  ( -60.00000000000000000, -37.00000000000000711, -20.00000000000000711 ) ) ;
#2749 = ORIENTED_EDGE ( 'NONE', *, *, #9020, .T. ) ;
#2750 = CLOSED_SHELL ( 'NONE', ( #11744, #13481, #12892, #14008, #15031, #2796, #9089, #7588, #7423, #3759, #9766, #4823, #3876, #5608, #14695, #5039, #451, #4544, #9312, #9707, #1419, #5923, #8038, #10795, #5536, #15578, #3060, #10962, #9054, #2447, #6622, #10571, #13675, #10631, #9499, #2491, #3085, #3960, #4359, #13345, #10515, #2520, #14408, #13001, #10591, #3464, #992 ) ) ;
#2751 = CARTESIAN_POINT ( 'NONE',  ( -55.00000000000000000, -5.000000000000000000, 0.000000000000000000 ) ) ;
#2752 = EDGE_CURVE ( 'NONE', #7410, #14039, #651, .T. ) ;
#2753 = AXIS2_PLACEMENT_3D ( 'NONE', #9504, #2212, #14892 ) ;
#2754 = CARTESIAN_POINT ( 'NONE',  ( -5.000000000000000888, -31.56250000000000000, -2.071067811865475949 ) ) ;
#2755 = ADVANCED_FACE ( 'NONE', ( #5575 ), #5013, .T. ) ;
#2756 = LINE ( 'NONE', #7623, #10042 ) ;
#2757 = DIRECTION ( 'NONE',  ( -0.000000000000000000, -1.000000000000000000, -0.000000000000000000 ) ) ;
#2758 = CARTESIAN_POINT ( 'NONE',  ( 1.415196051561583790, -4.795541693661363958, -0.2500000000000036637 ) ) ;
#2759 = APPLICATION_PROTOCOL_DEFINITION ( 'draft international standard', 'automotive_design', 1998, #327 ) ;
#2760 = CARTESIAN_POINT ( 'NONE',  ( 4.276409079477644148, 1.261996585732577891, -4.562499998634405252 ) ) ;
#2761 = SPHERICAL_SURFACE ( 'NONE', #5838, 10.00000000000000000 ) ;
#2762 = ORIENTED_EDGE ( 'NONE', *, *, #2, .T. ) ;
#2763 = CARTESIAN_POINT ( 'NONE',  ( 4.686969894964994943, -4.098233149437105816, -48.53786474802608097 ) ) ;
#2764 = ORIENTED_EDGE ( 'NONE', *, *, #15493, .F. ) ;
#2765 = FACE_OUTER_BOUND ( 'NONE', #8041, .T. ) ;
#2766 = AXIS2_PLACEMENT_3D ( 'NONE', #5472, #10403, #15573 ) ;
#2767 = DIRECTION ( 'NONE',  ( 0.000000000000000000, 1.000000000000000000, 0.000000000000000000 ) ) ;
#2768 = ORIENTED_EDGE ( 'NONE', *, *, #905, .F. ) ;
#2769 = ITEM_DEFINED_TRANSFORMATION ( 'NONE', 'NONE', #9921,  #3223 ) ;
#2770 = CARTESIAN_POINT ( 'NONE',  ( -3.753672977998669502, -3.033343224707661712, -5.999999998634408804 ) ) ;
#2771 = CARTESIAN_POINT ( 'NONE',  ( 0.5711823568785988625, 5.381735091635026613, -4.687499997268819385 ) ) ;
#2772 = EDGE_CURVE ( 'NONE', #7134, #5346, #13221, .T. ) ;
#2773 = ADVANCED_FACE ( 'NONE', ( #10597 ), #5656, .F. ) ;
#2774 = CARTESIAN_POINT ( 'NONE',  ( -2.071067811865492381, -28.43750000273118772, 4.999999999999985789 ) ) ;
#2775 = CIRCLE ( 'NONE', #12586, 3.499999999999999556 ) ;
#2776 = CARTESIAN_POINT ( 'NONE',  ( -3.750000000000007550, -6.495190528383289141, 0.000000000000000000 ) ) ;
#2777 = CARTESIAN_POINT ( 'NONE',  ( -3.333333333333335258, 2.694301256218251783, -3.300726591567079815 ) ) ;
#2778 = CARTESIAN_POINT ( 'NONE',  ( -0.5711823568785978633, -5.381735091635035495, -2.187499997268816720 ) ) ;
#2779 = CARTESIAN_POINT ( 'NONE',  ( 0.000000000000000000, -11.00000000000000178, -6.000000000000000888 ) ) ;
#2780 = APPLICATION_CONTEXT ( 'automotive_design' ) ;
#2781 = CARTESIAN_POINT ( 'NONE',  ( 19.99999999999956657, -8.786575603324269439E-13, -4.500000000000000000 ) ) ;
#2782 = DIRECTION ( 'NONE',  ( -0.000000000000000000, -1.000000000000000000, -0.000000000000000000 ) ) ;
#2783 = VERTEX_POINT ( 'NONE', #9372 ) ;
#2784 = DIRECTION ( 'NONE',  ( 0.000000000000000000, 0.000000000000000000, 1.000000000000000000 ) ) ;
#2785 = CARTESIAN_POINT ( 'NONE',  ( 3.916244202832140253, -2.131511515620588160, -7.437499998634407916 ) ) ;
#2786 = CIRCLE ( 'NONE', #6682, 2.499999999999998668 ) ;
#2787 = FACE_OUTER_BOUND ( 'NONE', #2245, .T. ) ;
#2788 = ORIENTED_EDGE ( 'NONE', *, *, #13644, .F. ) ;
#2789 = VERTEX_POINT ( 'NONE', #15521 ) ;
#2790 = VERTEX_POINT ( 'NONE', #3220 ) ;
#2791 = DIRECTION ( 'NONE',  ( 0.000000000000000000, 0.000000000000000000, -1.000000000000000000 ) ) ;
#2792 = AXIS2_PLACEMENT_3D ( 'NONE', #14224, #4368, #9302 ) ;
#2793 = FACE_OUTER_BOUND ( 'NONE', #15403, .T. ) ;
#2794 = VECTOR ( 'NONE', #975, 1000.000000000000000 ) ;
#2795 = DIRECTION ( 'NONE',  ( 0.000000000000000000, 0.000000000000000000, 1.000000000000000000 ) ) ;
#2796 = ADVANCED_FACE ( 'NONE', ( #8169 ), #13071, .F. ) ;
#2797 = CIRCLE ( 'NONE', #13897, 1.999999999999998224 ) ;
#2798 = CARTESIAN_POINT ( 'NONE',  ( 0.000000000000000000, -13.00000000000000178, -1.500000000000000000 ) ) ;
#2799 = CARTESIAN_POINT ( 'NONE',  ( 0.2791032213812760232, -8.821394357840572908, -7.929128246061912577 ) ) ;
#2800 = DIRECTION ( 'NONE',  ( -0.4999999999999965028, -0.8660254037844407060, 0.000000000000000000 ) ) ;
#2801 = CARTESIAN_POINT ( 'NONE',  ( -2.390265326283148806, -4.391654775818394363, -4.375000000000000000 ) ) ;
#2802 = DIRECTION ( 'NONE',  ( 0.000000000000000000, 0.000000000000000000, 1.000000000000000000 ) ) ;
#2803 = AXIS2_PLACEMENT_3D ( 'NONE', #10401, #5394, #6929 ) ;
#2804 = DIRECTION ( 'NONE',  ( 0.000000000000000000, 0.000000000000000000, 1.000000000000000000 ) ) ;
#2805 = CARTESIAN_POINT ( 'NONE',  ( -4.458734125000001214, -21.87500000136559208, 1.846868145590734089 ) ) ;
#2806 = AXIS2_PLACEMENT_3D ( 'NONE', #9851, #15693, #4925 ) ;
#2807 = CARTESIAN_POINT ( 'NONE',  ( 3.916244202832140253, -2.131511515620588160, -5.687499998634406140 ) ) ;
#2808 = VERTEX_POINT ( 'NONE', #883 ) ;
#2809 = CARTESIAN_POINT ( 'NONE',  ( -55.00000000000000000, 0.000000000000000000, 17.99999999999999289 ) ) ;
#2810 = VERTEX_POINT ( 'NONE', #5801 ) ;
#2811 = ORIENTED_EDGE ( 'NONE', *, *, #6309, .T. ) ;
#2812 = CARTESIAN_POINT ( 'NONE',  ( 1.846868145590735200, -30.50000000136559919, -4.458734125000000326 ) ) ;
#2813 = EDGE_CURVE ( 'NONE', #10194, #15230, #2321, .T. ) ;
#2814 = CARTESIAN_POINT ( 'NONE',  ( 17.00000000000000000, 0.000000000000000000, 0.000000000000000000 ) ) ;
#2815 = ORIENTED_EDGE ( 'NONE', *, *, #15378, .T. ) ;
#2816 = CARTESIAN_POINT ( 'NONE',  ( 0.5276280594147412240, -4.314175951381924889, -3.320322319201654881 ) ) ;
#2817 = AXIS2_PLACEMENT_3D ( 'NONE', #3973, #597, #10376 ) ;
#2818 = DIRECTION ( 'NONE',  ( 0.000000000000000000, 1.000000000000000000, -1.471414886128461471E-15 ) ) ;
#2819 = CARTESIAN_POINT ( 'NONE',  ( 1.261996585732578113, -4.276409079477644148, -2.562499998634407028 ) ) ;
#2820 = CARTESIAN_POINT ( 'NONE',  ( -35.00000000000000000, 40.00000000000000000, 0.000000000000000000 ) ) ;
#2821 = CARTESIAN_POINT ( 'NONE',  ( -5.000000000000000888, -29.43750000000000711, 2.071067811865474617 ) ) ;
#2822 = CARTESIAN_POINT ( 'NONE',  ( -44.43375672972994295, -5.000000000000000000, -20.00000000000000355 ) ) ;
#2823 = DIRECTION ( 'NONE',  ( 1.000000000000000000, 1.239088197126290324E-16, -0.000000000000000000 ) ) ;
#2824 = CARTESIAN_POINT ( 'NONE',  ( -5.000000000000000888, -22.68750000273119127, -2.071067811865475949 ) ) ;
#2825 = FACE_BOUND ( 'NONE', #13224, .T. ) ;
#2826 = CARTESIAN_POINT ( 'NONE',  ( -1.846868145590734756, -26.12500000136559564, -4.458734124999999437 ) ) ;
#2827 = CARTESIAN_POINT ( 'NONE',  ( 6.625705691649768525, -5.306270977113037191, -7.795653906408973377 ) ) ;
#2828 = ORIENTED_EDGE ( 'NONE', *, *, #15232, .F. ) ;
#2829 = ORIENTED_EDGE ( 'NONE', *, *, #12086, .F. ) ;
#2830 = B_SPLINE_CURVE_WITH_KNOTS ( 'NONE', 3,
 ( #15321, #13855, #12786, #6514, #11428, #375, #1730, #5293, #9030 ),
 .UNSPECIFIED., .F., .F.,
 ( 4, 2, 1, 2, 4 ),
 ( 0.000000000000000000, 0.002165063509461097498, 0.004330127018922194995, 0.006495190528383292493, 0.008660254037844389990 ),
 .UNSPECIFIED. ) ;
#2832 = ORIENTED_EDGE ( 'NONE', *, *, #4447, .F. ) ;
#2831 = EDGE_CURVE ( 'NONE', #11431, #513, #7590, .T. ) ;
#2833 = DIRECTION ( 'NONE',  ( 0.000000000000000000, 0.000000000000000000, 1.000000000000000000 ) ) ;
#2834 = EDGE_CURVE ( 'NONE', #434, #10287, #5541, .T. ) ;
#2835 = ORIENTED_EDGE ( 'NONE', *, *, #5189, .T. ) ;
#2836 = DIRECTION ( 'NONE',  ( -1.000000000000000000, -0.000000000000000000, -0.000000000000000000 ) ) ;
#2837 = DIRECTION ( 'NONE',  ( 0.000000000000000000, 0.4999999999999993339, -0.8660254037844390407 ) ) ;
#2838 = CARTESIAN_POINT ( 'NONE',  ( -8.190561711645485556E-16, -29.93750000136559564, 4.458734124999999437 ) ) ;
#2839 = CARTESIAN_POINT ( 'NONE',  ( -1.415196051561583790, 4.795541693661363958, -5.750000000000001776 ) ) ;
#2840 = CARTESIAN_POINT ( 'NONE',  ( -3.916244202832140253, 2.131511515620587272, -4.187499998634405252 ) ) ;
#2841 = DIRECTION ( 'NONE',  ( -0.000000000000000000, 1.000000000000000000, -0.000000000000000000 ) ) ;
#2842 = ORIENTED_EDGE ( 'NONE', *, *, #8040, .F. ) ;
#2843 = ORIENTED_EDGE ( 'NONE', *, *, #13459, .T. ) ;
#2844 = CARTESIAN_POINT ( 'NONE',  ( -5.000000000000002665, -1.404940523648820476E-14, -7.545263047592946748 ) ) ;
#2845 = CARTESIAN_POINT ( 'NONE',  ( -4.458734125000000326, -31.00000000136559564, -1.846868145590735644 ) ) ;
#2846 = ADVANCED_FACE ( 'NONE', ( #11127 ), #4761, .F. ) ;
#2847 = VERTEX_POINT ( 'NONE', #2554 ) ;
#2848 = CARTESIAN_POINT ( 'NONE',  ( -0.5093500532425060401, -4.799145180956616130, -7.874999998634408804 ) ) ;
#2849 = AXIS2_PLACEMENT_3D ( 'NONE', #10462, #4319, #9259 ) ;
#2850 = DIRECTION ( 'NONE',  ( 0.5000000000000013323, -0.8660254037844379305, 0.000000000000000000 ) ) ;
#2851 = DIRECTION ( 'NONE',  ( -1.000000000000000000, 0.000000000000000000, 0.000000000000000000 ) ) ;
#2852 = UNCERTAINTY_MEASURE_WITH_UNIT (LENGTH_MEASURE( 1.000000000000000082E-05 ), #5957, 'distance_accuracy_value', 'NONE');
#2853 = CARTESIAN_POINT ( 'NONE',  ( -4.209348295687703967, -3.401574460001763001, -3.312499997268815388 ) ) ;
#2854 = CARTESIAN_POINT ( 'NONE',  ( -1.415196051561583790, 4.795541693661363958, -8.624999997268814056 ) ) ;
#2855 = FILL_AREA_STYLE ('',( #7968 ) ) ;
#2856 = CARTESIAN_POINT ( 'NONE',  ( -4.458734124999999437, -22.25000000136559564, -1.846868145590735644 ) ) ;
#2857 = ORIENTED_EDGE ( 'NONE', *, *, #14089, .F. ) ;
#2858 = DIRECTION ( 'NONE',  ( 0.000000000000000000, 0.000000000000000000, 1.000000000000000000 ) ) ;
#2859 = LINE ( 'NONE', #1649, #5065 ) ;
#2860 = DIRECTION ( 'NONE',  ( 0.000000000000000000, -0.000000000000000000, 1.000000000000000000 ) ) ;
#2861 = ADVANCED_FACE ( 'NONE', ( #13531 ), #11717, .T. ) ;
#2862 = EDGE_LOOP ( 'NONE', ( #1575, #5938 ) ) ;
#2863 = DIRECTION ( 'NONE',  ( 0.000000000000000000, 1.000000000000000000, 0.000000000000000000 ) ) ;
#2864 = ORIENTED_EDGE ( 'NONE', *, *, #13988, .T. ) ;
#2865 = EDGE_CURVE ( 'NONE', #5376, #13100, #13225, .T. ) ;
#2866 = EDGE_CURVE ( 'NONE', #8315, #3368, #12331, .T. ) ;
#2867 = EDGE_CURVE ( 'NONE', #15384, #5460, #10678, .T. ) ;
#2868 = VERTEX_POINT ( 'NONE', #9911 ) ;
#2869 = CARTESIAN_POINT ( 'NONE',  ( 6.123233995736766282E-16, -20.00000000000000000, -5.000000000000000000 ) ) ;
#2870 = CARTESIAN_POINT ( 'NONE',  ( 42.02221399786069611, 0.000000000000000000, 1.040834085586084257E-13 ) ) ;
#2871 = DIRECTION ( 'NONE',  ( -0.000000000000000000, -1.000000000000000000, -0.000000000000000000 ) ) ;
#2872 = B_SPLINE_CURVE_WITH_KNOTS ( 'NONE', 3,
 ( #5428, #579, #5665, #10360, #14389, #9148, #1932, #10433 ),
 .UNSPECIFIED., .F., .F.,
 ( 4, 2, 2, 4 ),
 ( 0.000000000000000000, 0.002450665683189819262, 0.003675998524784728893, 0.004901331366379639391 ),
 .UNSPECIFIED. ) ;
#2873 = APPLICATION_CONTEXT ( 'automotive_design' ) ;
#2874 = FACE_OUTER_BOUND ( 'NONE', #3579, .T. ) ;
#2875 = CARTESIAN_POINT ( 'NONE',  ( -15.99999999999979217, -11.00000000000000178, -1.500000000000001110 ) ) ;
#2876 = CARTESIAN_POINT ( 'NONE',  ( -7.549004593702465016, -4.358419834287842853, -7.700121441565846325 ) ) ;
#2877 = CARTESIAN_POINT ( 'NONE',  ( -4.391654775818395251, 2.390265326283148806, -3.624999999999999556 ) ) ;
#2878 = FACE_OUTER_BOUND ( 'NONE', #15227, .T. ) ;
#2879 = CARTESIAN_POINT ( 'NONE',  ( 0.000000000000000000, -20.00000000000000000, -1.500000000000000000 ) ) ;
#2880 = CARTESIAN_POINT ( 'NONE',  ( -8.190561711645485556E-16, -23.68750000136559564, 4.458734124999999437 ) ) ;
#2881 = CARTESIAN_POINT ( 'NONE',  ( 4.276409079477644148, 1.261996585732577891, -8.562499998634409692 ) ) ;
#2882 = VERTEX_POINT ( 'NONE', #2237 ) ;
#2883 = UNCERTAINTY_MEASURE_WITH_UNIT (LENGTH_MEASURE( 1.000000000000000082E-05 ), #13339, 'distance_accuracy_value', 'NONE');
#2884 = FACE_OUTER_BOUND ( 'NONE', #12556, .T. ) ;
#2885 = VERTEX_POINT ( 'NONE', #3529 ) ;
#2886 = ORIENTED_EDGE ( 'NONE', *, *, #14291, .F. ) ;
#2887 = EDGE_CURVE ( 'NONE', #2626, #13323, #3142, .T. ) ;
#2888 = ORIENTED_EDGE ( 'NONE', *, *, #10649, .F. ) ;
#2889 = CARTESIAN_POINT ( 'NONE',  ( -4.458734125000000326, -29.25000000136559564, -1.846868145590735644 ) ) ;
#2890 = CARTESIAN_POINT ( 'NONE',  ( 0.000000000000000000, 0.000000000000000000, -4.484454397937119197 ) ) ;
#2891 = ORIENTED_EDGE ( 'NONE', *, *, #8811, .F. ) ;
#2892 = CARTESIAN_POINT ( 'NONE',  ( 0.000000000000000000, 0.000000000000000000, -25.03750572909317285 ) ) ;
#2893 = DIRECTION ( 'NONE',  ( 0.000000000000000000, 1.224646799147353207E-16, 1.000000000000000000 ) ) ;
#2894 = DIRECTION ( 'NONE',  ( -1.000000000000000000, -0.000000000000000000, -0.000000000000000000 ) ) ;
#2895 = LINE ( 'NONE', #12742, #12713 ) ;
#2896 = CARTESIAN_POINT ( 'NONE',  ( -2.071067811865478170, -30.31249999999999645, 5.000000000000000000 ) ) ;
#2897 = CARTESIAN_POINT ( 'NONE',  ( -3.033343224707664376, 3.753672977998667726, -4.999999998634407028 ) ) ;
#2898 = CYLINDRICAL_SURFACE ( 'NONE', #2132, 5.000000000000000888 ) ;
#2899 = DIRECTION ( 'NONE',  ( -1.000000000000000000, -0.000000000000000000, -0.000000000000000000 ) ) ;
#2900 = CARTESIAN_POINT ( 'NONE',  ( 3.535533905932736864, -26.25000000273118417, 3.535533905932738641 ) ) ;
#2901 = DIRECTION ( 'NONE',  ( 1.000000000000000000, 0.000000000000000000, 0.000000000000000000 ) ) ;
#2902 = CARTESIAN_POINT ( 'NONE',  ( 2.730187237215162345E-16, -25.18750000136559564, -4.458734124999999437 ) ) ;
#2903 = DIRECTION ( 'NONE',  ( 1.000000000000000000, 0.000000000000000000, 0.000000000000000000 ) ) ;
#2904 = ORIENTED_EDGE ( 'NONE', *, *, #15532, .F. ) ;
#2905 = ORIENTED_EDGE ( 'NONE', *, *, #7446, .F. ) ;
#2906 = EDGE_LOOP ( 'NONE', ( #14722, #12535, #546, #461 ) ) ;
#2907 = AXIS2_PLACEMENT_3D ( 'NONE', #14848, #8558, #3768 ) ;
#2908 = DIRECTION ( 'NONE',  ( 0.000000000000000000, 0.000000000000000000, 1.000000000000000000 ) ) ;
#2909 = ORIENTED_EDGE ( 'NONE', *, *, #9480, .T. ) ;
#2910 = PLANE ( 'NONE',  #3278 ) ;
#2911 = ADVANCED_BREP_SHAPE_REPRESENTATION ( '', ( #3697, #3223 ), #5534 ) ;
#2912 = DIRECTION ( 'NONE',  ( 0.000000000000000000, 0.000000000000000000, 1.000000000000000000 ) ) ;
#2913 = CARTESIAN_POINT ( 'NONE',  ( 3.152801135295366208, -29.81250000136559208, 3.152801135295367985 ) ) ;
#2914 = VECTOR ( 'NONE', #3639, 1000.000000000000000 ) ;
#2915 = CARTESIAN_POINT ( 'NONE',  ( 2.390265326283148806, 4.391654775818395251, -0.7499999972688138339 ) ) ;
#2916 = EDGE_CURVE ( 'NONE', #4240, #15626, #150, .T. ) ;
#2917 = CONTEXT_DEPENDENT_SHAPE_REPRESENTATION ( #3910, #4169 ) ;
#2918 = CARTESIAN_POINT ( 'NONE',  ( -0.5093500532425060401, -4.799145180956616130, -7.874999998634408804 ) ) ;
#2919 = CARTESIAN_POINT ( 'NONE',  ( -3.033343224707664376, 3.753672977998667726, -0.2499999986344070280 ) ) ;
#2920 = ORIENTED_EDGE ( 'NONE', *, *, #4424, .T. ) ;
#2921 = ORIENTED_EDGE ( 'NONE', *, *, #2127, .T. ) ;
#2922 = DIRECTION ( 'NONE',  ( 0.000000000000000000, -0.5000000000000012212, -0.8660254037844380415 ) ) ;
#2923 = CARTESIAN_POINT ( 'NONE',  ( 1.846868145590736310, -28.62500000136559919, 4.458734124999999437 ) ) ;
#2924 = EDGE_LOOP ( 'NONE', ( #7893, #9587, #3567, #3170 ) ) ;
#2925 =( LENGTH_UNIT ( ) NAMED_UNIT ( * ) SI_UNIT ( .MILLI., .METRE. ) );
#2926 = CARTESIAN_POINT ( 'NONE',  ( -5.000000000000004441, -1.011557177027151181E-15, -5.420263044861760804 ) ) ;
#2927 = EDGE_CURVE ( 'NONE', #13263, #6259, #15911, .T. ) ;
#2928 = LINE ( 'NONE', #1880, #7434 ) ;
#2929 = EDGE_CURVE ( 'NONE', #3228, #10093, #2390, .T. ) ;
#2930 = CARTESIAN_POINT ( 'NONE',  ( 4.795541693661363958, 1.415196051561583790, -7.874999997268816720 ) ) ;
#2931 = CARTESIAN_POINT ( 'NONE',  ( 0.000000000000000000, -32.00000000000000000, 5.000000000000000000 ) ) ;
#2932 = CARTESIAN_POINT ( 'NONE',  ( -36.99999999999999289, -11.00000000000000178, -1.999999999999170885 ) ) ;
#2933 = CARTESIAN_POINT ( 'NONE',  ( -1.846868145590737420, -23.00000000136559564, 4.458734124999997661 ) ) ;
#2934 = EDGE_LOOP ( 'NONE', ( #12396, #10392, #8390, #1023 ) ) ;
#2935 = CYLINDRICAL_SURFACE ( 'NONE', #15701, 10.00000000000000178 ) ;
#2936 = CARTESIAN_POINT ( 'NONE',  ( 0.5093500532425063732, 4.799145180956616130, -7.124999998634407916 ) ) ;
#2937 = DIRECTION ( 'NONE',  ( 0.000000000000000000, 1.000000000000000000, 0.000000000000000000 ) ) ;
#2938 = ORIENTED_EDGE ( 'NONE', *, *, #8366, .T. ) ;
#2939 = CARTESIAN_POINT ( 'NONE',  ( -4.000000000000000000, 0.8576368993457507139, -3.433240632782198709 ) ) ;
#2940 = ORIENTED_EDGE ( 'NONE', *, *, #335, .T. ) ;
#2941 =( BOUNDED_SURFACE ( )  B_SPLINE_SURFACE ( 1, 2, ( 
 ( #4132, #11481, #12443, #1377, #12523, #11244, #5108, #7712, #13660, #10044, #14977, #13983, #10367, #1467, #15297, #8999, #1625, #274, #5191, #428, #1550, #5353, #12608, #13911, #10291, #15052, #6653, #3966, #2838, #7789, #2913, #7864, #12762, #11562, #10760, #6806, #5591, #747, #5744, #13003, #14163, #5672, #10439, #10680, #901, #15376, #12848, #10610, #9237, #3092, #15611, #14398, #10528, #4453, #4532, #15538, #11951, #11637, #4210, #9466, #4298, #2999, #5823, #9155, #9317, #9388, #3325, #14312, #8276, #3241, #11875, #8188, #11711, #14238, #3160, #8032, #14072, #13167, #2027, #2103, #13088, #6890, #666, #11794, #6974, #1790, #821, #7047, #7949, #6735, #588, #5511, #12925, #1860, #15463, #4383, #8109, #1942, #3708, #11, #1207, #4928, #1123, #8655, #13553, #2486, #8344, #12184, #9612, #2339, #3635, #12354, #7128, #9856, #7447, #1286, #12266, #12030, #2177, #14548, #6231, #14787, #6152, #15697, #6063, #4613, #9546, #14473, #13240, #10992, #3468, #5984, #3395, #980, #5911, #10836, #15776, #4687, #7358, #14712, #8427, #13316, #13401, #15931, #2259, #7282, #7212, #4854, #12114, #1050, #11079, #13468, #10908, #15850, #4768, #9692, #14631, #3549, #8506, #9780, #8579 ),
 ( #2406, #8819, #7775, #13720, #6310, #6391, #15199, #9062, #6472, #11310, #1446, #15107, #5175, #4114, #13645, #11145, #11227, #5090, #5249, #10185, #172, #2574, #11462, #13964, #10025, #2653, #87, #2896, #5004, #7525, #11384, #10271, #1534, #12590, #3950, #8979, #3877, #7846, #336, #8739, #12744, #2821, #8895, #12666, #7604, #1688, #5333, #409, #260, #9932, #4027, #10104, #13891, #14961, #12503, #14871, #3793, #15036, #12428, #1361, #13798, #2736, #7692, #1606, #6547, #649, #10595, #10350, #11694, #6629, #14049, #9137, #570, #10659, #6956, #8166, #11857, #8090, #15592, #4511, #9446, #15277, #3143, #5491, #12908, #8257, #3303, #11542, #14376, #13149, #804, #14295, #5654, #494, #1770, #4365, #12984, #6717, #9299, #11620, #1920, #4191, #5418, #13068, #4435, #2975, #7929, #10421, #12826, #15356, #5572, #4275, #9217, #14139, #5724, #3069, #8012, #1843, #6868, #15519, #6786, #10509, #3218, #15443, #9370, #14222, #11775, #2006, #728, #3525, #9593, #8401, #1102, #12007, #7337, #9527, #6042, #8635, #4669, #3448, #14605, #3614, #10887, #959, #3526, #8328, #8559, #14766, #13218, #10737, #8480, #7106, #5884, #13448, #12242, #13292, #2319, #2388, #13381, #9834, #14456 ) ),
 .UNSPECIFIED., .F., .F., .F. ) 
 B_SPLINE_SURFACE_WITH_KNOTS ( ( 2, 2 ),
 ( 3, 2, 2, 2, 2, 2, 2, 2, 2, 2, 2, 2, 2, 2, 2, 2, 2, 2, 2, 2, 2, 2, 2, 2, 2, 2, 2, 2, 2, 2, 2, 2, 2, 2, 2, 2, 2, 2, 2, 2, 2, 2, 2, 2, 2, 2, 2, 2, 2, 2, 2, 2, 2, 2, 2, 2, 2, 2, 2, 2, 2, 2, 2, 2, 2, 2, 2, 2, 2, 2, 2, 2, 2, 2, 2, 2, 2, 2, 2, 2, 3 ),
 ( 0.000000000000000000, 1.000000000000000000 ),
 ( 0.000000000000000000, 0.01250000000000000069, 0.02500000000000000139, 0.03749999999999999861, 0.05000000000000000278, 0.06250000000000000000, 0.07499999999999999722, 0.08749999999999999445, 0.1000000000000000056, 0.1125000000000000028, 0.1250000000000000000, 0.1375000000000000111, 0.1499999999999999944, 0.1625000000000000056, 0.1749999999999999889, 0.1875000000000000000, 0.2000000000000000111, 0.2124999999999999944, 0.2250000000000000056, 0.2374999999999999889, 0.2500000000000000000, 0.2625000000000000111, 0.2750000000000000222, 0.2874999999999999778, 0.2999999999999999889, 0.3125000000000000000, 0.3250000000000000111, 0.3375000000000000222, 0.3499999999999999778, 0.3624999999999999889, 0.3750000000000000000, 0.3875000000000000111, 0.4000000000000000222, 0.4124999999999999778, 0.4249999999999999889, 0.4375000000000000000, 0.4500000000000000111, 0.4625000000000000222, 0.4749999999999999778, 0.4874999999999999889, 0.5000000000000000000, 0.5124999999999999556, 0.5250000000000000222, 0.5374999999999999778, 0.5500000000000000444, 0.5625000000000000000, 0.5749999999999999556, 0.5875000000000000222, 0.5999999999999999778, 0.6125000000000000444, 0.6250000000000000000, 0.6374999999999999556, 0.6500000000000000222, 0.6624999999999999778, 0.6750000000000000444, 0.6875000000000000000, 0.6999999999999999556, 0.7125000000000000222, 0.7249999999999999778, 0.7375000000000000444, 0.7500000000000000000, 0.7624999999999999556, 0.7750000000000000222, 0.7874999999999999778, 0.8000000000000000444, 0.8125000000000000000, 0.8249999999999999556, 0.8375000000000000222, 0.8499999999999999778, 0.8625000000000000444, 0.8750000000000000000, 0.8874999999999999556, 0.9000000000000000222, 0.9124999999999999778, 0.9250000000000000444, 0.9375000000000000000, 0.9499999999999999556, 0.9625000000000000222, 0.9749999999999999778, 0.9875000000000000444, 1.000000000000000000 ),
 .UNSPECIFIED. ) 
 GEOMETRIC_REPRESENTATION_ITEM ( )  RATIONAL_B_SPLINE_SURFACE ( (
 ( 1.000000000000000000, 0.9238795325112867385, 1.000000000000000000, 0.9238795325112867385, 1.000000000000000000, 0.9238795325112867385, 1.000000000000000000, 0.9238795325112867385, 1.000000000000000000, 0.9238795325112867385, 1.000000000000000000, 0.9238795325112867385, 1.000000000000000000, 0.9238795325112867385, 1.000000000000000000, 0.9238795325112867385, 1.000000000000000000, 0.9238795325112867385, 1.000000000000000000, 0.9238795325112867385, 1.000000000000000000, 0.9238795325112867385, 1.000000000000000000, 0.9238795325112867385, 1.000000000000000000, 0.9238795325112867385, 1.000000000000000000, 0.9238795325112867385, 1.000000000000000000, 0.9238795325112867385, 1.000000000000000000, 0.9238795325112867385, 1.000000000000000000, 0.9238795325112867385, 1.000000000000000000, 0.9238795325112867385, 1.000000000000000000, 0.9238795325112867385, 1.000000000000000000, 0.9238795325112867385, 1.000000000000000000, 0.9238795325112867385, 1.000000000000000000, 0.9238795325112867385, 1.000000000000000000, 0.9238795325112867385, 1.000000000000000000, 0.9238795325112867385, 1.000000000000000000, 0.9238795325112867385, 1.000000000000000000, 0.9238795325112867385, 1.000000000000000000, 0.9238795325112867385, 1.000000000000000000, 0.9238795325112867385, 1.000000000000000000, 0.9238795325112867385, 1.000000000000000000, 0.9238795325112867385, 1.000000000000000000, 0.9238795325112867385, 1.000000000000000000, 0.9238795325112867385, 1.000000000000000000, 0.9238795325112867385, 1.000000000000000000, 0.9238795325112867385, 1.000000000000000000, 0.9238795325112867385, 1.000000000000000000, 0.9238795325112867385, 1.000000000000000000, 0.9238795325112867385, 1.000000000000000000, 0.9238795325112867385, 1.000000000000000000, 0.9238795325112867385, 1.000000000000000000, 0.9238795325112867385, 1.000000000000000000, 0.9238795325112867385, 1.000000000000000000, 0.9238795325112867385, 1.000000000000000000, 0.9238795325112867385, 1.000000000000000000, 0.9238795325112867385, 1.000000000000000000, 0.9238795325112867385, 1.000000000000000000, 0.9238795325112867385, 1.000000000000000000, 0.9238795325112867385, 1.000000000000000000, 0.9238795325112867385, 1.000000000000000000, 0.9238795325112867385, 1.000000000000000000, 0.9238795325112867385, 1.000000000000000000, 0.9238795325112867385, 1.000000000000000000, 0.9238795325112867385, 1.000000000000000000, 0.9238795325112867385, 1.000000000000000000, 0.9238795325112867385, 1.000000000000000000, 0.9238795325112867385, 1.000000000000000000, 0.9238795325112867385, 1.000000000000000000, 0.9238795325112867385, 1.000000000000000000, 0.9238795325112867385, 1.000000000000000000, 0.9238795325112867385, 1.000000000000000000, 0.9238795325112867385, 1.000000000000000000, 0.9238795325112867385, 1.000000000000000000, 0.9238795325112867385, 1.000000000000000000, 0.9238795325112867385, 1.000000000000000000, 0.9238795325112867385, 1.000000000000000000, 0.9238795325112867385, 1.000000000000000000, 0.9238795325112867385, 1.000000000000000000, 0.9238795325112867385, 1.000000000000000000, 0.9238795325112867385, 1.000000000000000000, 0.9238795325112867385, 1.000000000000000000, 0.9238795325112867385, 1.000000000000000000, 0.9238795325112867385, 1.000000000000000000, 0.9238795325112867385, 1.000000000000000000, 0.9238795325112867385, 1.000000000000000000, 0.9238795325112867385, 1.000000000000000000, 0.9238795325112867385, 1.000000000000000000, 0.9238795325112867385, 1.000000000000000000, 0.9238795325112867385, 1.000000000000000000, 0.9238795325112867385, 1.000000000000000000, 0.9238795325112867385, 1.000000000000000000, 0.9238795325112867385, 1.000000000000000000),
 ( 1.000000000000000000, 0.9238795325112867385, 1.000000000000000000, 0.9238795325112867385, 1.000000000000000000, 0.9238795325112867385, 1.000000000000000000, 0.9238795325112867385, 1.000000000000000000, 0.9238795325112867385, 1.000000000000000000, 0.9238795325112867385, 1.000000000000000000, 0.9238795325112867385, 1.000000000000000000, 0.9238795325112867385, 1.000000000000000000, 0.9238795325112867385, 1.000000000000000000, 0.9238795325112867385, 1.000000000000000000, 0.9238795325112867385, 1.000000000000000000, 0.9238795325112867385, 1.000000000000000000, 0.9238795325112867385, 1.000000000000000000, 0.9238795325112867385, 1.000000000000000000, 0.9238795325112867385, 1.000000000000000000, 0.9238795325112867385, 1.000000000000000000, 0.9238795325112867385, 1.000000000000000000, 0.9238795325112867385, 1.000000000000000000, 0.9238795325112867385, 1.000000000000000000, 0.9238795325112867385, 1.000000000000000000, 0.9238795325112867385, 1.000000000000000000, 0.9238795325112867385, 1.000000000000000000, 0.9238795325112867385, 1.000000000000000000, 0.9238795325112867385, 1.000000000000000000, 0.9238795325112867385, 1.000000000000000000, 0.9238795325112867385, 1.000000000000000000, 0.9238795325112867385, 1.000000000000000000, 0.9238795325112867385, 1.000000000000000000, 0.9238795325112867385, 1.000000000000000000, 0.9238795325112867385, 1.000000000000000000, 0.9238795325112867385, 1.000000000000000000, 0.9238795325112867385, 1.000000000000000000, 0.9238795325112867385, 1.000000000000000000, 0.9238795325112867385, 1.000000000000000000, 0.9238795325112867385, 1.000000000000000000, 0.9238795325112867385, 1.000000000000000000, 0.9238795325112867385, 1.000000000000000000, 0.9238795325112867385, 1.000000000000000000, 0.9238795325112867385, 1.000000000000000000, 0.9238795325112867385, 1.000000000000000000, 0.9238795325112867385, 1.000000000000000000, 0.9238795325112867385, 1.000000000000000000, 0.9238795325112867385, 1.000000000000000000, 0.9238795325112867385, 1.000000000000000000, 0.9238795325112867385, 1.000000000000000000, 0.9238795325112867385, 1.000000000000000000, 0.9238795325112867385, 1.000000000000000000, 0.9238795325112867385, 1.000000000000000000, 0.9238795325112867385, 1.000000000000000000, 0.9238795325112867385, 1.000000000000000000, 0.9238795325112867385, 1.000000000000000000, 0.9238795325112867385, 1.000000000000000000, 0.9238795325112867385, 1.000000000000000000, 0.9238795325112867385, 1.000000000000000000, 0.9238795325112867385, 1.000000000000000000, 0.9238795325112867385, 1.000000000000000000, 0.9238795325112867385, 1.000000000000000000, 0.9238795325112867385, 1.000000000000000000, 0.9238795325112867385, 1.000000000000000000, 0.9238795325112867385, 1.000000000000000000, 0.9238795325112867385, 1.000000000000000000, 0.9238795325112867385, 1.000000000000000000, 0.9238795325112867385, 1.000000000000000000, 0.9238795325112867385, 1.000000000000000000, 0.9238795325112867385, 1.000000000000000000, 0.9238795325112867385, 1.000000000000000000, 0.9238795325112867385, 1.000000000000000000, 0.9238795325112867385, 1.000000000000000000, 0.9238795325112867385, 1.000000000000000000, 0.9238795325112867385, 1.000000000000000000, 0.9238795325112867385, 1.000000000000000000, 0.9238795325112867385, 1.000000000000000000, 0.9238795325112867385, 1.000000000000000000, 0.9238795325112867385, 1.000000000000000000, 0.9238795325112867385, 1.000000000000000000, 0.9238795325112867385, 1.000000000000000000, 0.9238795325112867385, 1.000000000000000000, 0.9238795325112867385, 1.000000000000000000, 0.9238795325112867385, 1.000000000000000000, 0.9238795325112867385, 1.000000000000000000) ) ) 
 REPRESENTATION_ITEM ( '' )  SURFACE ( )  );
#2942 = VECTOR ( 'NONE', #7108, 1000.000000000000000 ) ;
#2943 = ORIENTED_EDGE ( 'NONE', *, *, #12398, .T. ) ;
#2944 = CARTESIAN_POINT ( 'NONE',  ( -55.00000000000000000, -5.000000000000000000, 0.000000000000000000 ) ) ;
#2945 = FACE_OUTER_BOUND ( 'NONE', #968, .T. ) ;
#2946 = CARTESIAN_POINT ( 'NONE',  ( 0.2500000000000002220, 4.898587196589412829E-16, -4.000000000000000000 ) ) ;
#2947 = AXIS2_PLACEMENT_3D ( 'NONE', #15631, #995, #2116 ) ;
#2948 = EDGE_CURVE ( 'NONE', #4422, #13155, #14768, .T. ) ;
#2949 = CARTESIAN_POINT ( 'NONE',  ( 5.000000000000000000, -26.18750000273118772, 2.071067811865478614 ) ) ;
#2950 = CARTESIAN_POINT ( 'NONE',  ( -21.01110699893060030, -3.000000000000001332, 39.04230484541322710 ) ) ;
#2951 = ADVANCED_FACE ( 'NONE', ( #2878 ), #11603, .T. ) ;
#2952 = CIRCLE ( 'NONE', #131, 2.041999999999999815 ) ;
#2953 = DIRECTION ( 'NONE',  ( 0.8660254037844383745, -0.000000000000000000, 0.5000000000000004441 ) ) ;
#2954 = CARTESIAN_POINT ( 'NONE',  ( 4.795541693661363958, 1.415196051561583790, -4.000000000000000000 ) ) ;
#2955 = CARTESIAN_POINT ( 'NONE',  ( -9.184850993605147944E-16, -30.25000000000000000, 5.000000000000000000 ) ) ;
#2956 = CARTESIAN_POINT ( 'NONE',  ( -5.040301471719076609, -5.750234626350518852, -0.09933465333851491941 ) ) ;
#2957 = CARTESIAN_POINT ( 'NONE',  ( 4.458734124999999437, -24.43750000136559564, 0.000000000000000000 ) ) ;
#2958 = CARTESIAN_POINT ( 'NONE',  ( -3.916244202832140253, 2.131511515620587272, -5.187499998634406140 ) ) ;
#2959 = EDGE_LOOP ( 'NONE', ( #4836, #7640, #283, #1936 ) ) ;
#2960 = CYLINDRICAL_SURFACE ( 'NONE', #681, 75.00000000000004263 ) ;
#2961 = ORIENTED_EDGE ( 'NONE', *, *, #600, .F. ) ;
#2962 = ORIENTED_EDGE ( 'NONE', *, *, #4129, .T. ) ;
#2963 = PRESENTATION_LAYER_ASSIGNMENT (  '', '', ( #14323 ) ) ;
#2964 = AXIS2_PLACEMENT_3D ( 'NONE', #1966, #2049, #9699 ) ;
#2965 = ORIENTED_EDGE ( 'NONE', *, *, #12944, .F. ) ;
#2966 = CARTESIAN_POINT ( 'NONE',  ( -1.846868145590734756, -30.37500000136559564, -4.458734125000000326 ) ) ;
#2967 = DIRECTION ( 'NONE',  ( 0.000000000000000000, -1.000000000000000000, 0.000000000000000000 ) ) ;
#2968 = CIRCLE ( 'NONE', #11735, 3.499999999999999556 ) ;
#2969 = ORIENTED_EDGE ( 'NONE', *, *, #4658, .T. ) ;
#2970 = LINE ( 'NONE', #7919, #10951 ) ;
#2971 = CARTESIAN_POINT ( 'NONE',  ( 7.500000000000000000, 3.160172554975060333, -7.231829826456837473 ) ) ;
#2972 = CARTESIAN_POINT ( 'NONE',  ( 3.916244202832140253, -2.131511515620588160, -6.437499998634407028 ) ) ;
#2973 = CARTESIAN_POINT ( 'NONE',  ( 67.49999999999931788, 37.00000000000000000, 2.650000000000013678 ) ) ;
#2974 = EDGE_CURVE ( 'NONE', #3368, #8728, #10973, .T. ) ;
#2975 = CARTESIAN_POINT ( 'NONE',  ( -5.000000000000000888, -25.43750000000000355, 2.071067811865474617 ) ) ;
#2976 = CIRCLE ( 'NONE', #8422, 25.00000000000000000 ) ;
#2977 = CARTESIAN_POINT ( 'NONE',  ( -1.261996585732579224, 4.276409079477648589, -5.062499998634406140 ) ) ;
#2978 = DIRECTION ( 'NONE',  ( 0.000000000000000000, 0.000000000000000000, 1.000000000000000000 ) ) ;
#2979 = DIRECTION ( 'NONE',  ( 0.000000000000000000, 0.000000000000000000, 1.000000000000000000 ) ) ;
#2980 = CARTESIAN_POINT ( 'NONE',  ( -2.071067811865478170, -23.43750000273119127, 5.000000000000000000 ) ) ;
#2981 = CIRCLE ( 'NONE', #1434, 6.000000000000000888 ) ;
#2982 = CARTESIAN_POINT ( 'NONE',  ( 4.729367062499999719, -21.28125000204839168, 0.000000000000000000 ) ) ;
#2983 = CIRCLE ( 'NONE', #7129, 4.999999999999997335 ) ;
#2984 = CARTESIAN_POINT ( 'NONE',  ( -3.152801135295367096, -25.06250000136559564, -3.152801135295367541 ) ) ;
#2985 = CARTESIAN_POINT ( 'NONE',  ( -5.000000000000002665, -1.404940523648820476E-14, -6.545263047592945860 ) ) ;
#2986 = ORIENTED_EDGE ( 'NONE', *, *, #3942, .F. ) ;
#2987 = ORIENTED_EDGE ( 'NONE', *, *, #641, .F. ) ;
#2988 = DIRECTION ( 'NONE',  ( 0.000000000000000000, -1.000000000000000000, 0.000000000000000000 ) ) ;
#2989 = VERTEX_POINT ( 'NONE', #15260 ) ;
#2990 = CARTESIAN_POINT ( 'NONE',  ( 7.500000000000000000, 4.330127018922190096, -7.422398894150031623 ) ) ;
#2991 = CIRCLE ( 'NONE', #6612, 2.649999999999985700 ) ;
#2992 = ORIENTED_EDGE ( 'NONE', *, *, #892, .F. ) ;
#2993 = FACE_OUTER_BOUND ( 'NONE', #3292, .T. ) ;
#2994 = AXIS2_PLACEMENT_3D ( 'NONE', #11453, #13957, #3785 ) ;
#2995 =( REPRESENTATION_RELATIONSHIP ('NONE','NONE', #4176, #10906 ) REPRESENTATION_RELATIONSHIP_WITH_TRANSFORMATION ( #2769 )SHAPE_REPRESENTATION_RELATIONSHIP( ) );
#2996 = DIRECTION ( 'NONE',  ( 0.4999999999999998890, 0.000000000000000000, 0.8660254037844387076 ) ) ;
#2997 = B_SPLINE_CURVE_WITH_KNOTS ( 'NONE', 3,
 ( #12779, #15554, #15312, #8046, #13020, #1721 ),
 .UNSPECIFIED., .F., .F.,
 ( 4, 2, 4 ),
 ( 0.002365888236227967761, 0.003551327329835077609, 0.004736766423442186590 ),
 .UNSPECIFIED. ) ;
#2998 = EDGE_CURVE ( 'NONE', #15426, #15162, #1749, .T. ) ;
#2999 = CARTESIAN_POINT ( 'NONE',  ( 1.846868145590736310, -27.87500000136559564, 4.458734124999999437 ) ) ;
#3000 = CARTESIAN_POINT ( 'NONE',  ( -3.401574460001765221, 4.209348295687701302, -6.562499997268814944 ) ) ;
#3001 = VECTOR ( 'NONE', #9161, 1000.000000000000000 ) ;
#3002 = PLANE ( 'NONE',  #12312 ) ;
#3003 = CARTESIAN_POINT ( 'NONE',  ( 5.000000000000000000, -31.12500000273118772, 0.000000000000000000 ) ) ;
#3004 = B_SPLINE_CURVE_WITH_KNOTS ( 'NONE', 3,
 ( #9935, #6065, #13556, #982, #14874 ),
 .UNSPECIFIED., .F., .F.,
 ( 4, 1, 4 ),
 ( 0.000000000000000000, 0.002309401076758505356, 0.004618802153517010713 ),
 .UNSPECIFIED. ) ;
#3005 = ORIENTED_EDGE ( 'NONE', *, *, #1011, .F. ) ;
#3006 = AXIS2_PLACEMENT_3D ( 'NONE', #7750, #12644, #8791 ) ;
#3007 = ORIENTED_EDGE ( 'NONE', *, *, #7190, .F. ) ;
#3008 = DIRECTION ( 'NONE',  ( 1.000000000000000000, 0.000000000000000000, 0.000000000000000000 ) ) ;
#3009 = CARTESIAN_POINT ( 'NONE',  ( 3.152801135295367541, -30.31250000136559564, -3.152801135295367541 ) ) ;
#3010 = ORIENTED_EDGE ( 'NONE', *, *, #13000, .T. ) ;
#3011 = ADVANCED_FACE ( 'NONE', ( #5473 ), #14003, .T. ) ;
#3012 = VECTOR ( 'NONE', #7245, 1000.000000000000000 ) ;
#3013 = CARTESIAN_POINT ( 'NONE',  ( -15.99999999999979217, -9.000000000000001776, -1.500000000000001110 ) ) ;
#3014 = PRODUCT_DEFINITION_FORMATION_WITH_SPECIFIED_SOURCE ( 'ANY', '', #8362, .NOT_KNOWN. ) ;
#3015 = CONICAL_SURFACE ( 'NONE', #3789, 7.500000000000001776, 0.8594454914424796144 ) ;
#3016 = DIRECTION ( 'NONE',  ( 0.000000000000000000, 0.000000000000000000, 1.000000000000000000 ) ) ;
#3017 = CARTESIAN_POINT ( 'NONE',  ( 19.99999999999956657, -8.786575603324269439E-13, 1.500000000000000000 ) ) ;
#3018 = UNCERTAINTY_MEASURE_WITH_UNIT (LENGTH_MEASURE( 1.000000000000000082E-05 ), #13477, 'distance_accuracy_value', 'NONE');
#3019 = CARTESIAN_POINT ( 'NONE',  ( 0.5711823568785989735, 5.381735091635026613, -7.687499997268816720 ) ) ;
#3020 = DIRECTION ( 'NONE',  ( 0.000000000000000000, 0.000000000000000000, 1.000000000000000000 ) ) ;
#3021 = VECTOR ( 'NONE', #13757, 1000.000000000000000 ) ;
#3022 = CARTESIAN_POINT ( 'NONE',  ( -60.00000000000000000, -37.00000000000000711, 19.99999999999999289 ) ) ;
#3023 = ORIENTED_EDGE ( 'NONE', *, *, #780, .T. ) ;
#3024 = DIRECTION ( 'NONE',  ( 0.000000000000000000, 0.000000000000000000, 1.000000000000000000 ) ) ;
#3025 = CARTESIAN_POINT ( 'NONE',  ( 2.500000000000000000, -1.178949249685213863, 2.042000000000002924 ) ) ;
#3026 = CARTESIAN_POINT ( 'NONE',  ( -3.535533905932737309, -26.75000000273118772, -3.535533905932738197 ) ) ;
#3027 = ORIENTED_EDGE ( 'NONE', *, *, #5041, .T. ) ;
#3028 = CARTESIAN_POINT ( 'NONE',  ( -4.211399284164270895, 2.459729995988205964, -3.751162237960538715 ) ) ;
#3029 = ORIENTED_EDGE ( 'NONE', *, *, #925, .T. ) ;
#3030 = ORIENTED_EDGE ( 'NONE', *, *, #14261, .F. ) ;
#3031 = AXIS2_PLACEMENT_3D ( 'NONE', #2944, #2791, #11360 ) ;
#3032 = CARTESIAN_POINT ( 'NONE',  ( -6.765421556309547668E-13, 40.00000000000000000, 67.49999999999930367 ) ) ;
#3033 = EDGE_CURVE ( 'NONE', #10280, #14464, #11078, .T. ) ;
#3034 = FACE_OUTER_BOUND ( 'NONE', #10178, .T. ) ;
#3035 = EDGE_CURVE ( 'NONE', #5346, #10287, #3930, .T. ) ;
#3036 = CARTESIAN_POINT ( 'NONE',  ( -7.500000000000001776, 0.000000000000000000, 0.000000000000000000 ) ) ;
#3037 = VECTOR ( 'NONE', #9374, 1000.000000000000000 ) ;
#3038 = B_SPLINE_CURVE_WITH_KNOTS ( 'NONE', 3,
 ( #8252, #13503, #2440, #14822, #1396, #2298, #5043, #8776 ),
 .UNSPECIFIED., .F., .F.,
 ( 4, 2, 2, 4 ),
 ( 2.465131517071352357E-07, 0.001183067374689843057, 0.001774477805458910071, 0.002365888236227977302 ),
 .UNSPECIFIED. ) ;
#3039 = MECHANICAL_DESIGN_GEOMETRIC_PRESENTATION_REPRESENTATION (  '', ( #3506 ), #6368 ) ;
#3040 = DIRECTION ( 'NONE',  ( -0.000000000000000000, 1.000000000000000000, -0.000000000000000000 ) ) ;
#3041 = FACE_OUTER_BOUND ( 'NONE', #8493, .T. ) ;
#3042 = CARTESIAN_POINT ( 'NONE',  ( -7.808218555863024157, -4.508077085118360472, -7.999534413642737540 ) ) ;
#3043 = CIRCLE ( 'NONE', #14152, 75.00000000000001421 ) ;
#3044 = CARTESIAN_POINT ( 'NONE',  ( 0.000000000000000000, 0.000000000000000000, 0.000000000000000000 ) ) ;
#3045 = CARTESIAN_POINT ( 'NONE',  ( 0.000000000000000000, -1.178949249685213863, 2.042000000000002924 ) ) ;
#3046 = DIRECTION ( 'NONE',  ( 0.5000000000000002220, 0.000000000000000000, -0.8660254037844383745 ) ) ;
#3047 = CARTESIAN_POINT ( 'NONE',  ( -4.458734124999999437, -23.93750000136559564, -5.460374474430324690E-16 ) ) ;
#3048 =( BOUNDED_CURVE ( )  B_SPLINE_CURVE ( 2, ( #7088, #9283, #13276, #6936, #5710, #5869, #8235, #9580, #15504, #3129, #4496, #8313, #940, #9509, #3365, #7172, #4654, #8386, #10722, #11990, #5636, #9431, #15579, #3432, #14359, #5951, #10802, #13202, #2141, #3288, #15656, #15742, #14205, #2218, #11841, #13133, #14511, #2069, #12074, #4420, #8073, #12969, #1018, #15423, #4574, #4345, #9355, #7013, #1904, #788, #6850, #14441, #14280, #11915, #11757, #711, #10579, #3202, #8151, #13048, #1988, #863, #5783, #9980, #13511, #7487, #10871, #12151, #3508, #1248, #4814, #7405, #14919, #12309, #5050, #6196, #2533, #9894, #2374, #11524, #4895, #13365, #1088, #15893, #7251, #14831, #4967, #51, #8466, #11113, #3839, #13434, #1165, #8546, #8782, #2306, #1405, #6028, #9820, #2615, #13684, #10950, #7569, #9736, #3672, #3750, #12466, #8698, #7322, #14587, #15813, #14674, #13601, #3599, #6109, #4730, #9651, #12224, #11036, #14749, #8619, #2449, #12390, #1326, #6270, #11184, #129, #9177, #15318, #11425, #453, #12873, #11270, #11586, #5375, #6678, #538, #15070, #12551, #2933, #10231, #13930, #15243, #12631, #10317, #3912, #4152, #12783, #9098, #6351, #14099, #2856, #7811, #5455, #6511, #218, #1646, #372, #11501, #5211, #10146 ),
 .UNSPECIFIED., .F., .F. ) 
 B_SPLINE_CURVE_WITH_KNOTS ( ( 3, 2, 2, 2, 2, 2, 2, 2, 2, 2, 2, 2, 2, 2, 2, 2, 2, 2, 2, 2, 2, 2, 2, 2, 2, 2, 2, 2, 2, 2, 2, 2, 2, 2, 2, 2, 2, 2, 2, 2, 2, 2, 2, 2, 2, 2, 2, 2, 2, 2, 2, 2, 2, 2, 2, 2, 2, 2, 2, 2, 2, 2, 2, 2, 2, 2, 2, 2, 2, 2, 2, 2, 2, 2, 2, 2, 2, 2, 2, 2, 3 ),
 ( 0.000000000000000000, 0.01250000000000000069, 0.02500000000000000139, 0.03749999999999999861, 0.05000000000000000278, 0.06250000000000000000, 0.07499999999999999722, 0.08749999999999999445, 0.1000000000000000056, 0.1125000000000000028, 0.1250000000000000000, 0.1375000000000000111, 0.1499999999999999944, 0.1625000000000000056, 0.1749999999999999889, 0.1875000000000000000, 0.2000000000000000111, 0.2124999999999999944, 0.2250000000000000056, 0.2374999999999999889, 0.2500000000000000000, 0.2625000000000000111, 0.2750000000000000222, 0.2874999999999999778, 0.2999999999999999889, 0.3125000000000000000, 0.3250000000000000111, 0.3375000000000000222, 0.3499999999999999778, 0.3624999999999999889, 0.3750000000000000000, 0.3875000000000000111, 0.4000000000000000222, 0.4124999999999999778, 0.4249999999999999889, 0.4375000000000000000, 0.4500000000000000111, 0.4625000000000000222, 0.4749999999999999778, 0.4874999999999999889, 0.5000000000000000000, 0.5124999999999999556, 0.5250000000000000222, 0.5374999999999999778, 0.5500000000000000444, 0.5625000000000000000, 0.5749999999999999556, 0.5875000000000000222, 0.5999999999999999778, 0.6125000000000000444, 0.6250000000000000000, 0.6374999999999999556, 0.6500000000000000222, 0.6624999999999999778, 0.6750000000000000444, 0.6875000000000000000, 0.6999999999999999556, 0.7125000000000000222, 0.7249999999999999778, 0.7375000000000000444, 0.7500000000000000000, 0.7624999999999999556, 0.7750000000000000222, 0.7874999999999999778, 0.8000000000000000444, 0.8125000000000000000, 0.8249999999999999556, 0.8375000000000000222, 0.8499999999999999778, 0.8625000000000000444, 0.8750000000000000000, 0.8874999999999999556, 0.9000000000000000222, 0.9124999999999999778, 0.9250000000000000444, 0.9375000000000000000, 0.9499999999999999556, 0.9625000000000000222, 0.9749999999999999778, 0.9875000000000000444, 1.000000000000000000 ),
 .UNSPECIFIED. ) 
 CURVE ( )  GEOMETRIC_REPRESENTATION_ITEM ( )  RATIONAL_B_SPLINE_CURVE ( ( 1.000000000000000000, 0.9238795325112867385, 1.000000000000000000, 0.9238795325112867385, 1.000000000000000000, 0.9238795325112867385, 1.000000000000000000, 0.9238795325112867385, 1.000000000000000000, 0.9238795325112867385, 1.000000000000000000, 0.9238795325112867385, 1.000000000000000000, 0.9238795325112867385, 1.000000000000000000, 0.9238795325112867385, 1.000000000000000000, 0.9238795325112867385, 1.000000000000000000, 0.9238795325112867385, 1.000000000000000000, 0.9238795325112867385, 1.000000000000000000, 0.9238795325112867385, 1.000000000000000000, 0.9238795325112867385, 1.000000000000000000, 0.9238795325112867385, 1.000000000000000000, 0.9238795325112867385, 1.000000000000000000, 0.9238795325112867385, 1.000000000000000000, 0.9238795325112867385, 1.000000000000000000, 0.9238795325112867385, 1.000000000000000000, 0.9238795325112867385, 1.000000000000000000, 0.9238795325112867385, 1.000000000000000000, 0.9238795325112867385, 1.000000000000000000, 0.9238795325112867385, 1.000000000000000000, 0.9238795325112867385, 1.000000000000000000, 0.9238795325112867385, 1.000000000000000000, 0.9238795325112867385, 1.000000000000000000, 0.9238795325112867385, 1.000000000000000000, 0.9238795325112867385, 1.000000000000000000, 0.9238795325112867385, 1.000000000000000000, 0.9238795325112867385, 1.000000000000000000, 0.9238795325112867385, 1.000000000000000000, 0.9238795325112867385, 1.000000000000000000, 0.9238795325112867385, 1.000000000000000000, 0.9238795325112867385, 1.000000000000000000, 0.9238795325112867385, 1.000000000000000000, 0.9238795325112867385, 1.000000000000000000, 0.9238795325112867385, 1.000000000000000000, 0.9238795325112867385, 1.000000000000000000, 0.9238795325112867385, 1.000000000000000000, 0.9238795325112867385, 1.000000000000000000, 0.9238795325112867385, 1.000000000000000000, 0.9238795325112867385, 1.000000000000000000, 0.9238795325112867385, 1.000000000000000000, 0.9238795325112867385, 1.000000000000000000, 0.9238795325112867385, 1.000000000000000000, 0.9238795325112867385, 1.000000000000000000, 0.9238795325112867385, 1.000000000000000000, 0.9238795325112867385, 1.000000000000000000, 0.9238795325112867385, 1.000000000000000000, 0.9238795325112867385, 1.000000000000000000, 0.9238795325112867385, 1.000000000000000000, 0.9238795325112867385, 1.000000000000000000, 0.9238795325112867385, 1.000000000000000000, 0.9238795325112867385, 1.000000000000000000, 0.9238795325112867385, 1.000000000000000000, 0.9238795325112867385, 1.000000000000000000, 0.9238795325112867385, 1.000000000000000000, 0.9238795325112867385, 1.000000000000000000, 0.9238795325112867385, 1.000000000000000000, 0.9238795325112867385, 1.000000000000000000, 0.9238795325112867385, 1.000000000000000000, 0.9238795325112867385, 1.000000000000000000, 0.9238795325112867385, 1.000000000000000000, 0.9238795325112867385, 1.000000000000000000, 0.9238795325112867385, 1.000000000000000000, 0.9238795325112867385, 1.000000000000000000, 0.9238795325112867385, 1.000000000000000000, 0.9238795325112867385, 1.000000000000000000, 0.9238795325112867385, 1.000000000000000000, 0.9238795325112867385, 1.000000000000000000, 0.9238795325112867385, 1.000000000000000000, 0.9238795325112867385, 1.000000000000000000, 0.9238795325112867385, 1.000000000000000000, 0.9238795325112867385, 1.000000000000000000, 0.9238795325112867385, 1.000000000000000000, 0.9238795325112867385, 1.000000000000000000, 0.9238795325112867385, 1.000000000000000000, 0.9238795325112867385, 1.000000000000000000, 0.9238795325112867385, 1.000000000000000000, 0.9238795325112867385, 1.000000000000000000, 0.9238795325112867385, 1.000000000000000000 ) ) 
 REPRESENTATION_ITEM ( '' )  );
#3049 = SHAPE_REPRESENTATION ( 'Mounting Flange Plate', ( #3223 ), #15373 ) ;
#3050 = CARTESIAN_POINT ( 'NONE',  ( 3.753672977998667726, 3.033343224707664376, -7.499999998634409692 ) ) ;
#3051 = ORIENTED_EDGE ( 'NONE', *, *, #1378, .F. ) ;
#3052 = COLOUR_RGB ( '', 0.40784314, 0.44705882, 0.49803922) ;
#3053 = EDGE_LOOP ( 'NONE', ( #931, #14779 ) ) ;
#3054 = CARTESIAN_POINT ( 'NONE',  ( -4.240553267258006517E-16, 9.016154170237607346, -7.999534413642735764 ) ) ;
#3055 = ORIENTED_EDGE ( 'NONE', *, *, #4930, .F. ) ;
#3056 = ORIENTED_EDGE ( 'NONE', *, *, #3832, .T. ) ;
#3057 =( NAMED_UNIT ( * ) PLANE_ANGLE_UNIT ( ) SI_UNIT ( $, .RADIAN. ) );
#3058 = CARTESIAN_POINT ( 'NONE',  ( 4.458734125000000326, -29.62500000136559208, -1.846868145590734978 ) ) ;
#3059 = CARTESIAN_POINT ( 'NONE',  ( -2.449848172108560540, -3.432307619358754724, -3.503702292528910078 ) ) ;
#3060 = ADVANCED_FACE ( 'NONE', ( #554 ), #6696, .T. ) ;
#3061 = VERTEX_POINT ( 'NONE', #10404 ) ;
#3062 = AXIS2_PLACEMENT_3D ( 'NONE', #4477, #4324, #8131 ) ;
#3063 = DIRECTION ( 'NONE',  ( 0.000000000000000000, 0.000000000000000000, 1.000000000000000000 ) ) ;
#3064 = CARTESIAN_POINT ( 'NONE',  ( 14.41154273188008439, -5.000000000000004441, 60.96152422706632024 ) ) ;
#3065 = CARTESIAN_POINT ( 'NONE',  ( -1.261996585732579224, 4.276409079477648589, -4.062499998634405252 ) ) ;
#3066 = FACE_OUTER_BOUND ( 'NONE', #14680, .T. ) ;
#3067 = CONICAL_SURFACE ( 'NONE', #2521, 10.39117206796836079, 1.221730476396047926 ) ;
#3068 = AXIS2_PLACEMENT_3D ( 'NONE', #6714, #11615, #8163 ) ;
#3069 = CARTESIAN_POINT ( 'NONE',  ( 2.071067811865475505, -24.81250000000000000, -5.000000000000000888 ) ) ;
#3070 = CARTESIAN_POINT ( 'NONE',  ( 2.131511515620586383, 3.916244202832140253, -8.187499998634407916 ) ) ;
#3071 = CARTESIAN_POINT ( 'NONE',  ( -3.679171394226034675, -2.494631558665844739, -0.3503314178412558211 ) ) ;
#3072 = CARTESIAN_POINT ( 'NONE',  ( 19.99999999999956657, -8.786575603324269439E-13, -4.500000000000000000 ) ) ;
#3073 = CARTESIAN_POINT ( 'NONE',  ( -2.071067811865478170, -25.43750000273118772, 5.000000000000000000 ) ) ;
#3074 = EDGE_LOOP ( 'NONE', ( #6900, #3628 ) ) ;
#3075 = AXIS2_PLACEMENT_3D ( 'NONE', #7314, #8612, #1239 ) ;
#3076 = CARTESIAN_POINT ( 'NONE',  ( -3.152801135295367985, -27.81250000136559564, 3.152801135295367096 ) ) ;
#3077 = LINE ( 'NONE', #14148, #10986 ) ;
#3078 = ORIENTED_EDGE ( 'NONE', *, *, #9985, .F. ) ;
#3079 = ORIENTED_EDGE ( 'NONE', *, *, #14190, .T. ) ;
#3080 = CARTESIAN_POINT ( 'NONE',  ( -7.922798540899434805, 4.627424769998857990, -8.057412477672054152 ) ) ;
#3082 = EDGE_CURVE ( 'NONE', #3405, #3174, #7066, .T. ) ;
#3081 = ORIENTED_EDGE ( 'NONE', *, *, #4447, .T. ) ;
#3083 = CARTESIAN_POINT ( 'NONE',  ( -43.93709122729256222, -3.012258285427890758, 21.74438836017856147 ) ) ;
#3084 = AXIS2_PLACEMENT_3D ( 'NONE', #8510, #89, #5006 ) ;
#3085 = ADVANCED_FACE ( 'NONE', ( #9119 ), #11367, .T. ) ;
#3086 = EDGE_CURVE ( 'NONE', #1929, #3803, #1109, .T. ) ;
#3087 = CIRCLE ( 'NONE', #256, 2.649999999999992806 ) ;
#3088 = EDGE_CURVE ( 'NONE', #6007, #4880, #12453, .T. ) ;
#3089 = ORIENTED_EDGE ( 'NONE', *, *, #5802, .F. ) ;
#3090 = DIRECTION ( 'NONE',  ( -1.000000000000000000, 0.000000000000000000, 0.000000000000000000 ) ) ;
#3091 = DIRECTION ( 'NONE',  ( 6.938893903907228378E-16, 1.000000000000000000, -0.000000000000000000 ) ) ;
#3092 = CARTESIAN_POINT ( 'NONE',  ( 4.458734125000000326, -28.62500000136559919, -1.846868145590734978 ) ) ;
#3093 = CARTESIAN_POINT ( 'NONE',  ( 5.000000000000004441, -2.247904837838113790E-16, -6.045263047592945860 ) ) ;
#3094 = CARTESIAN_POINT ( 'NONE',  ( -4.795541693661363958, -1.415196051561583790, -0.3749999972688169980 ) ) ;
#3095 = APPLICATION_PROTOCOL_DEFINITION ( 'draft international standard', 'automotive_design', 1998, #11438 ) ;
#3096 = CARTESIAN_POINT ( 'NONE',  ( -4.999999999999847233, 1.272547481429013860, -7.461597479913464781 ) ) ;
#3097 = AXIS2_PLACEMENT_3D ( 'NONE', #4641, #2205, #8299 ) ;
#3098 = CARTESIAN_POINT ( 'NONE',  ( -4.799145180956616130, 0.5093500532425063732, 0.8750000013655920839 ) ) ;
#3099 = EDGE_LOOP ( 'NONE', ( #3078, #14226, #5732, #14176, #2642 ) ) ;
#3100 = ORIENTED_EDGE ( 'NONE', *, *, #5391, .T. ) ;
#3101 = CARTESIAN_POINT ( 'NONE',  ( -34.99999999999999289, -13.00000000000000178, -1.999999999999170441 ) ) ;
#3102 = EDGE_CURVE ( 'NONE', #12397, #3134, #14026, .T. ) ;
#3103 = ORIENTED_EDGE ( 'NONE', *, *, #6192, .F. ) ;
#3104 =( REPRESENTATION_RELATIONSHIP ('NONE','NONE', #4176, #396 ) REPRESENTATION_RELATIONSHIP_WITH_TRANSFORMATION ( #9081 )SHAPE_REPRESENTATION_RELATIONSHIP( ) );
#3105 = VECTOR ( 'NONE', #11656, 1000.000000000000000 ) ;
#3106 = CARTESIAN_POINT ( 'NONE',  ( -5.000000000000004441, -1.011557177027151181E-15, -4.545263047592944083 ) ) ;
#3107 = DIRECTION ( 'NONE',  ( 0.000000000000000000, -1.000000000000000000, 0.000000000000000000 ) ) ;
#3108 = DIRECTION ( 'NONE',  ( -1.000000000000000000, -0.000000000000000000, -0.000000000000000000 ) ) ;
#3109 = CARTESIAN_POINT ( 'NONE',  ( -4.391654775818395251, 2.390265326283148806, -8.499999997268814056 ) ) ;
#3110 = DIRECTION ( 'NONE',  ( 1.000000000000000000, 0.000000000000000000, 0.000000000000000000 ) ) ;
#3111 = CARTESIAN_POINT ( 'NONE',  ( 4.000000000000000000, 2.309401076758515803, -0.4999999999999995559 ) ) ;
#3112 = ORIENTED_EDGE ( 'NONE', *, *, #5162, .F. ) ;
#3113 = CARTESIAN_POINT ( 'NONE',  ( -28.86751345948129455, -4.999999999999997335, 22.00000000000000711 ) ) ;
#3114 = CARTESIAN_POINT ( 'NONE',  ( -7.922281120364393914, 4.573931137438272287, -8.047472243342932430 ) ) ;
#3115 = EDGE_LOOP ( 'NONE', ( #5621, #10954 ) ) ;
#3116 = DIRECTION ( 'NONE',  ( -1.000000000000000000, 1.734723475976808080E-16, 0.000000000000000000 ) ) ;
#3117 = ORIENTED_EDGE ( 'NONE', *, *, #15732, .T. ) ;
#3118 = VERTEX_POINT ( 'NONE', #10334 ) ;
#3119 = CARTESIAN_POINT ( 'NONE',  ( 17.99999999999957012, -8.784126309725975241E-13, -4.500000000000000000 ) ) ;
#3120 = FACE_OUTER_BOUND ( 'NONE', #4526, .T. ) ;
#3121 = CARTESIAN_POINT ( 'NONE',  ( -7.500000000000004441, 1.489914625144000304, -0.1187923833806791979 ) ) ;
#3122 = CARTESIAN_POINT ( 'NONE',  ( -28.86751345948126257, -20.00000000000000000, -50.00000000000000711 ) ) ;
#3123 = CARTESIAN_POINT ( 'NONE',  ( -3.535533905932737309, -25.62500000000000355, -3.535533905932738197 ) ) ;
#3124 = CARTESIAN_POINT ( 'NONE',  ( -9.184850993605147944E-16, -26.25000000000000355, 5.000000000000000000 ) ) ;
#3125 = LINE ( 'NONE', #10644, #10930 ) ;
#3126 = EDGE_CURVE ( 'NONE', #8883, #7552, #11755, .T. ) ;
#3127 = DIRECTION ( 'NONE',  ( 0.000000000000000000, 0.000000000000000000, -1.000000000000000000 ) ) ;
#3128 = EDGE_CURVE ( 'NONE', #11629, #13499, #4252, .T. ) ;
#3129 = CARTESIAN_POINT ( 'NONE',  ( -4.458734125000000326, -31.12500000136559564, 1.846868145590734089 ) ) ;
#3130 = CARTESIAN_POINT ( 'NONE',  ( 3.753672977998667726, 3.033343224707664376, 0.7500000013655939712 ) ) ;
#3131 = VERTEX_POINT ( 'NONE', #707 ) ;
#3132 = DIRECTION ( 'NONE',  ( -1.000000000000000000, -0.000000000000000000, -0.000000000000000000 ) ) ;
#3133 = VERTEX_POINT ( 'NONE', #5634 ) ;
#3134 = VERTEX_POINT ( 'NONE', #10577 ) ;
#3135 = CARTESIAN_POINT ( 'NONE',  ( -1.846868145590737420, -27.00000000136559208, 4.458734124999999437 ) ) ;
#3136 = DIRECTION ( 'NONE',  ( 0.9396926207859143121, 1.150791560227857665E-16, -0.3420201433256525592 ) ) ;
#3137 = ORIENTED_EDGE ( 'NONE', *, *, #10177, .F. ) ;
#3138 = CARTESIAN_POINT ( 'NONE',  ( 67.49999999999931788, 40.00000000000000000, 2.081668171172168513E-14 ) ) ;
#3139 = CARTESIAN_POINT ( 'NONE',  ( 7.499999999999999112, 4.652409454067510275, -7.929128589908465585 ) ) ;
#3140 = CARTESIAN_POINT ( 'NONE',  ( 3.916244202832140253, -2.131511515620588160, -3.437499998634407916 ) ) ;
#3141 = DIRECTION ( 'NONE',  ( 0.000000000000000000, 0.000000000000000000, 1.000000000000000000 ) ) ;
#3142 =( BOUNDED_CURVE ( )  B_SPLINE_CURVE ( 2, ( #10889, #7193, #14851, #6130, #8717, #6044, #12093, #7507, #12408, #1342, #4750 ),
 .UNSPECIFIED., .F., .F. ) 
 B_SPLINE_CURVE_WITH_KNOTS ( ( 3, 2, 2, 2, 2, 3 ),
 ( 0.5545872658012773737, 0.5625000000000000000, 0.5749999999999999556, 0.5875000000000000222, 0.5999999999999999778, 0.6045872658012773071 ),
 .UNSPECIFIED. ) 
 CURVE ( )  GEOMETRIC_REPRESENTATION_ITEM ( )  RATIONAL_B_SPLINE_CURVE ( ( 0.9646335149384803742, 0.9518143178943441196, 1.000000000000000000, 0.9238795325112867385, 1.000000000000000000, 0.9238795325112867385, 1.000000000000000000, 0.9238795325112867385, 1.000000000000000000, 0.9720652146169428409, 0.9646335149384808183 ) ) 
 REPRESENTATION_ITEM ( '' )  );
#3143 = CARTESIAN_POINT ( 'NONE',  ( 3.535533905932738197, -26.87500000000000000, -3.535533905932738197 ) ) ;
#3144 = CARTESIAN_POINT ( 'NONE',  ( -4.276409079477644148, -1.261996585732578335, -5.812499998634406140 ) ) ;
#3145 = DIRECTION ( 'NONE',  ( 0.000000000000000000, 1.000000000000000000, 0.000000000000000000 ) ) ;
#3146 = EDGE_CURVE ( 'NONE', #3781, #7386, #938, .T. ) ;
#3147 = LINE ( 'NONE', #10598, #6660 ) ;
#3148 = EDGE_CURVE ( 'NONE', #8470, #3419, #12891, .T. ) ;
#3149 = CARTESIAN_POINT ( 'NONE',  ( -3.535533905932737309, -24.75000000273118417, -3.535533905932738197 ) ) ;
#3150 = ORIENTED_EDGE ( 'NONE', *, *, #15289, .T. ) ;
#3151 = CARTESIAN_POINT ( 'NONE',  ( -3.152801135295367985, -25.81250000136559564, 3.152801135295367096 ) ) ;
#3152 = CARTESIAN_POINT ( 'NONE',  ( 1.249327701958355741, -8.410337540185093275, -7.776713651266290661 ) ) ;
#3153 = ORIENTED_EDGE ( 'NONE', *, *, #7920, .T. ) ;
#3154 = VERTEX_POINT ( 'NONE', #4343 ) ;
#3155 = CARTESIAN_POINT ( 'NONE',  ( -7.500000000000003553, 3.202583086486119779, -7.213046687579564242 ) ) ;
#3156 = CARTESIAN_POINT ( 'NONE',  ( 43.08845726811992449, 0.000000000000000000, -38.63139720814411504 ) ) ;
#3157 = VERTEX_POINT ( 'NONE', #2139 ) ;
#3158 = CARTESIAN_POINT ( 'NONE',  ( 3.061616997868383141E-16, -30.75000000000000000, -5.000000000000000000 ) ) ;
#3159 = CARTESIAN_POINT ( 'NONE',  ( 40.98096197215471648, -3.000000000000000000, -26.98110827881998119 ) ) ;
#3160 = CARTESIAN_POINT ( 'NONE',  ( -3.152801135295367985, -27.06250000136559564, 3.152801135295367096 ) ) ;
#3161 = CARTESIAN_POINT ( 'NONE',  ( 0.5636800770130377947, 4.293361309317166530, -3.531542292954102713 ) ) ;
#3162 = EDGE_CURVE ( 'NONE', #12752, #4331, #6296, .T. ) ;
#3163 = CARTESIAN_POINT ( 'NONE',  ( -55.00000000000000000, -5.000000000000000000, -18.00000000000001066 ) ) ;
#3164 = EDGE_CURVE ( 'NONE', #10935, #4422, #7069, .T. ) ;
#3165 = CONTEXT_DEPENDENT_SHAPE_REPRESENTATION ( #9695, #3439 ) ;
#3166 = CIRCLE ( 'NONE', #2648, 6.000000000000000888 ) ;
#3167 = CARTESIAN_POINT ( 'NONE',  ( -4.276409079477644148, -1.261996585732578335, -8.062499998634407916 ) ) ;
#3168 = DIRECTION ( 'NONE',  ( -1.000000000000000000, -0.000000000000000000, -0.000000000000000000 ) ) ;
#3169 = TOROIDAL_SURFACE ( 'NONE', #5505, 27.99999999999998934, 2.000000000000000000 ) ;
#3170 = ORIENTED_EDGE ( 'NONE', *, *, #7879, .F. ) ;
#3171 = VERTEX_POINT ( 'NONE', #11913 ) ;
#3172 = SPHERICAL_SURFACE ( 'NONE', #8273, 10.00000000000000000 ) ;
#3173 = SHAPE_REPRESENTATION ( 'hex flange nut gradea 1_iso_ISO - 4161 - M10 - N', ( #3223 ), #7084 ) ;
#3174 = VERTEX_POINT ( 'NONE', #9508 ) ;
#3175 = CIRCLE ( 'NONE', #12189, 39.99999999999999289 ) ;
#3176 = CARTESIAN_POINT ( 'NONE',  ( 0.5711823568785988625, 5.381735091635026613, -4.812500000000000000 ) ) ;
#3177 = CIRCLE ( 'NONE', #13737, 5.999999999999991118 ) ;
#3178 = CARTESIAN_POINT ( 'NONE',  ( -28.86751345948126612, -35.00000000000000000, -18.00000000000000355 ) ) ;
#3179 = CARTESIAN_POINT ( 'NONE',  ( 2.500000000000000000, 0.000000000000000000, 0.000000000000000000 ) ) ;
#3180 = EDGE_CURVE ( 'NONE', #15384, #3645, #14357, .T. ) ;
#3182 = VECTOR ( 'NONE', #7339, 1000.000000000000000 ) ;
#3181 = CARTESIAN_POINT ( 'NONE',  ( -2.390265326283148806, -4.391654775818394363, -8.249999997268814056 ) ) ;
#3183 = CARTESIAN_POINT ( 'NONE',  ( 0.000000000000000000, -20.00000000000000000, -5.000000000000000000 ) ) ;
#3184 = CARTESIAN_POINT ( 'NONE',  ( 5.000000000000000888, 0.000000000000000000, -25.03750572909317285 ) ) ;
#3185 = DIRECTION ( 'NONE',  ( -1.000000000000000000, -0.000000000000000000, -0.000000000000000000 ) ) ;
#3186 = ORIENTED_EDGE ( 'NONE', *, *, #12580, .F. ) ;
#3187 = CARTESIAN_POINT ( 'NONE',  ( -28.86751345948130165, 88.59290746114278647, 18.00000000000000355 ) ) ;
#3188 = CARTESIAN_POINT ( 'NONE',  ( -55.00000000000000000, -5.000000000000000000, 17.99999999999999289 ) ) ;
#3189 = ORIENTED_EDGE ( 'NONE', *, *, #585, .F. ) ;
#3190 = DIRECTION ( 'NONE',  ( -0.000000000000000000, -1.000000000000000000, -0.000000000000000000 ) ) ;
#3191 = VERTEX_POINT ( 'NONE', #5708 ) ;
#3192 = ORIENTED_EDGE ( 'NONE', *, *, #4801, .T. ) ;
#3193 = DIRECTION ( 'NONE',  ( 0.4999999999999997224, 0.000000000000000000, 0.8660254037844387076 ) ) ;
#3194 = FACE_OUTER_BOUND ( 'NONE', #2089, .T. ) ;
#3195 = CARTESIAN_POINT ( 'NONE',  ( -124.9999999999999716, -10.00000000000001066, 7.500000000000001776 ) ) ;
#3196 = CARTESIAN_POINT ( 'NONE',  ( -28.86751345948129455, -4.999999999999997335, 49.99999999999999289 ) ) ;
#3197 = DIRECTION ( 'NONE',  ( -0.000000000000000000, 1.000000000000000000, -0.000000000000000000 ) ) ;
#3198 = CARTESIAN_POINT ( 'NONE',  ( 4.458734124998676052, -0.1932007455631602477, -0.3789984458506766019 ) ) ;
#3199 = CARTESIAN_POINT ( 'NONE',  ( -2.886751345948139758, -37.00000000000000711, 35.00000000000000000 ) ) ;
#3200 = DIRECTION ( 'NONE',  ( -0.000000000000000000, -1.000000000000000000, -0.000000000000000000 ) ) ;
#3201 = FACE_OUTER_BOUND ( 'NONE', #15843, .T. ) ;
#3202 = CARTESIAN_POINT ( 'NONE',  ( -4.458734125000000326, -28.12500000136559564, 1.846868145590734089 ) ) ;
#3203 = CARTESIAN_POINT ( 'NONE',  ( 1.261996585732578113, -4.276409079477644148, -1.562499998634406140 ) ) ;
#3204 = ORIENTED_EDGE ( 'NONE', *, *, #8662, .F. ) ;
#3205 = UNCERTAINTY_MEASURE_WITH_UNIT (LENGTH_MEASURE( 1.000000000000000082E-05 ), #8747, 'distance_accuracy_value', 'NONE');
#3206 = CARTESIAN_POINT ( 'NONE',  ( -60.00000000000000000, 0.000000000000000000, -20.00000000000000711 ) ) ;
#3207 = EDGE_LOOP ( 'NONE', ( #10502, #9474, #7054, #6299, #10765 ) ) ;
#3208 = ORIENTED_EDGE ( 'NONE', *, *, #15815, .F. ) ;
#3209 = CARTESIAN_POINT ( 'NONE',  ( 4.458734124999999437, -27.68750000136559564, 0.000000000000000000 ) ) ;
#3210 = CARTESIAN_POINT ( 'NONE',  ( -4.211140560182196957, -2.431303136016552013, -3.745885042887436178 ) ) ;
#3211 = AXIS2_PLACEMENT_3D ( 'NONE', #6279, #11043, #14839 ) ;
#3212 = CARTESIAN_POINT ( 'NONE',  ( -2.390265326283148806, -4.391654775818394363, -6.375000000000001776 ) ) ;
#3213 = EDGE_CURVE ( 'NONE', #4719, #4136, #14277, .T. ) ;
#3214 = AXIS2_PLACEMENT_3D ( 'NONE', #3999, #15168, #8711 ) ;
#3215 = CARTESIAN_POINT ( 'NONE',  ( -44.43375672974056556, -5.000000000000000000, 20.00000000000000000 ) ) ;
#3216 = CARTESIAN_POINT ( 'NONE',  ( 3.033343224707661712, -3.753672977998669502, -3.499999998634409692 ) ) ;
#3217 = DIRECTION ( 'NONE',  ( 0.000000000000000000, 0.000000000000000000, 1.000000000000000000 ) ) ;
#3218 = CARTESIAN_POINT ( 'NONE',  ( -3.535533905932738641, -24.37500000000000000, 3.535533905932737309 ) ) ;
#3219 = CARTESIAN_POINT ( 'NONE',  ( -3.401574460001764777, 4.209348295687701302, 1.312499999999996447 ) ) ;
#3220 = CARTESIAN_POINT ( 'NONE',  ( -34.99999999999999289, -11.00000000000000178, -1.999999999999170441 ) ) ;
#3221 = DIRECTION ( 'NONE',  ( 1.000000000000000000, 0.000000000000000000, 0.000000000000000000 ) ) ;
#3222 = CARTESIAN_POINT ( 'NONE',  ( 2.730187237215162345E-16, -29.18750000136559208, -4.458734124999999437 ) ) ;
#3223 = AXIS2_PLACEMENT_3D ( 'NONE', #11897, #11972, #4638 ) ;
#3224 = ORIENTED_EDGE ( 'NONE', *, *, #1439, .T. ) ;
#3225 = VECTOR ( 'NONE', #8211, 1000.000000000000000 ) ;
#3226 = CYLINDRICAL_SURFACE ( 'NONE', #1487, 5.000000000000000000 ) ;
#3227 = PLANE ( 'NONE',  #6600 ) ;
#3228 = VERTEX_POINT ( 'NONE', #14203 ) ;
#3229 = VERTEX_POINT ( 'NONE', #10485 ) ;
#3231 = CARTESIAN_POINT ( 'NONE',  ( -4.999999999999849898, 1.272547481429008309, -3.461597479913464781 ) ) ;
#3230 = AXIS2_PLACEMENT_3D ( 'NONE', #10329, #7502, #11515 ) ;
#3232 = CARTESIAN_POINT ( 'NONE',  ( -5.725490332106780933, 0.000000000000000000, -9.916840153467775920 ) ) ;
#3233 = EDGE_LOOP ( 'NONE', ( #11734, #9232 ) ) ;
#3234 = DIRECTION ( 'NONE',  ( -0.000000000000000000, 1.000000000000000000, -0.000000000000000000 ) ) ;
#3235 = EDGE_CURVE ( 'NONE', #15957, #1169, #3125, .T. ) ;
#3236 = ADVANCED_FACE ( 'NONE', ( #1986 ), #786, .F. ) ;
#3237 =( BOUNDED_CURVE ( )  B_SPLINE_CURVE ( 2, ( #10790, #11667, #3274, #4485, #5543, #14268, #11978, #12883, #10475 ),
 .UNSPECIFIED., .F., .F. ) 
 B_SPLINE_CURVE_WITH_KNOTS ( ( 3, 2, 2, 2, 3 ),
 ( 0.1250000000000001110, 0.1375000000000001221, 0.1500000000000001332, 0.1625000000000001443, 0.1750000000000001554 ),
 .UNSPECIFIED. ) 
 CURVE ( )  GEOMETRIC_REPRESENTATION_ITEM ( )  RATIONAL_B_SPLINE_CURVE ( ( 0.9999999999999993339, 0.9238795325112874046, 1.000000000000000000, 0.9238795325112867385, 1.000000000000000000, 0.9238795325112867385, 1.000000000000000000, 0.9238795325112857393, 1.000000000000001110 ) ) 
 REPRESENTATION_ITEM ( '' )  );
#3238 = AXIS2_PLACEMENT_3D ( 'NONE', #193, #12336, #7344 ) ;
#3239 = DIRECTION ( 'NONE',  ( 0.000000000000000000, 1.000000000000000000, -0.000000000000000000 ) ) ;
#3240 = PRESENTATION_LAYER_ASSIGNMENT (  '', '', ( #12508 ) ) ;
#3241 = CARTESIAN_POINT ( 'NONE',  ( -1.846868145590734756, -27.37500000136559564, -4.458734125000000326 ) ) ;
#3242 = DIRECTION ( 'NONE',  ( 1.000000000000000000, 0.000000000000000000, 0.000000000000000000 ) ) ;
#3243 = CARTESIAN_POINT ( 'NONE',  ( 2.500000000000000000, 2.357898499370433054, -1.951563910473907981E-15 ) ) ;
#3244 = DIRECTION ( 'NONE',  ( -1.000000000000000000, -0.000000000000000000, -0.000000000000000000 ) ) ;
#3245 = CARTESIAN_POINT ( 'NONE',  ( -4.336808689942017736E-16, -8.660254037844399733, -7.422398894150038728 ) ) ;
#3246 = DIRECTION ( 'NONE',  ( 0.000000000000000000, 0.000000000000000000, 1.000000000000000000 ) ) ;
#3247 = ORIENTED_EDGE ( 'NONE', *, *, #15306, .T. ) ;
#3248 = AXIS2_PLACEMENT_3D ( 'NONE', #15818, #3291, #793 ) ;
#3249 = ORIENTED_EDGE ( 'NONE', *, *, #2018, .T. ) ;
#3250 = DIRECTION ( 'NONE',  ( 0.000000000000000000, 0.000000000000000000, 1.000000000000000000 ) ) ;
#3251 = VECTOR ( 'NONE', #3540, 1000.000000000000000 ) ;
#3252 = ORIENTED_EDGE ( 'NONE', *, *, #10570, .T. ) ;
#3253 = AXIS2_PLACEMENT_3D ( 'NONE', #3138, #8007, #14453 ) ;
#3254 = ADVANCED_FACE ( 'NONE', ( #5867 ), #15574, .F. ) ;
#3255 = EDGE_CURVE ( 'NONE', #3401, #5290, #15711, .T. ) ;
#3256 = CYLINDRICAL_SURFACE ( 'NONE', #6862, 2.000000000000000888 ) ;
#3257 = CARTESIAN_POINT ( 'NONE',  ( -4.795541693661363958, -1.415196051561583790, -3.374999997268816276 ) ) ;
#3258 = CARTESIAN_POINT ( 'NONE',  ( -3.753672977998669946, -3.033343224707661712, 1.250000001365594304 ) ) ;
#3259 = AXIS2_PLACEMENT_3D ( 'NONE', #3682, #4583, #2228 ) ;
#3260 = CARTESIAN_POINT ( 'NONE',  ( -4.209348295687703967, -3.401574460001763001, -6.312499997268814056 ) ) ;
#3261 = CLOSED_SHELL ( 'NONE', ( #3737, #8881, #9193, #3011, #2755, #15614, #5700, #9905, #1878, #12640, #6913, #15117, #13782, #7901, #9643, #11723, #15235, #6986, #6620, #1682, #1298, #15595, #8679, #8814, #13135, #10346, #10652, #12433, #2366, #2846, #5245, #15947 ) ) ;
#3262 = CARTESIAN_POINT ( 'NONE',  ( -21.01110699893041911, -3.000000000000001332, -39.04230484541332657 ) ) ;
#3263 = LINE ( 'NONE', #15636, #10301 ) ;
#3264 = DIRECTION ( 'NONE',  ( 1.000000000000000000, -0.000000000000000000, 1.114413700119375779E-16 ) ) ;
#3265 = EDGE_LOOP ( 'NONE', ( #1274, #6914, #6984, #8682 ) ) ;
#3266 = CARTESIAN_POINT ( 'NONE',  ( -35.00000000000000000, 50.00000000000000000, 2.649999999999985700 ) ) ;
#3267 = CARTESIAN_POINT ( 'NONE',  ( -4.391654775818395251, 2.390265326283148806, -2.499999997268815388 ) ) ;
#3268 = SURFACE_STYLE_USAGE ( .BOTH. , #7154 ) ;
#3269 = VERTEX_POINT ( 'NONE', #12966 ) ;
#3270 = CYLINDRICAL_SURFACE ( 'NONE', #6972, 2.649999999999985700 ) ;
#3271 = AXIS2_PLACEMENT_3D ( 'NONE', #13828, #3168, #4215 ) ;
#3272 = ORIENTED_EDGE ( 'NONE', *, *, #8123, .T. ) ;
#3273 = ORIENTED_EDGE ( 'NONE', *, *, #2238, .T. ) ;
#3274 = CARTESIAN_POINT ( 'NONE',  ( -3.535533905932737309, -30.62500000000000000, -3.535533905932738197 ) ) ;
#3275 = EDGE_CURVE ( 'NONE', #10300, #9472, #15960, .T. ) ;
#3276 = CARTESIAN_POINT ( 'NONE',  ( -39.99999999999999289, -9.000000000000001776, 8.300651832549021947E-13 ) ) ;
#3277 = CIRCLE ( 'NONE', #15707, 2.499999999999998668 ) ;
#3278 = AXIS2_PLACEMENT_3D ( 'NONE', #6733, #15049, #1621 ) ;
#3279 = ADVANCED_FACE ( 'NONE', ( #2067 ), #1902, .F. ) ;
#3280 = VECTOR ( 'NONE', #15141, 1000.000000000000000 ) ;
#3281 = CARTESIAN_POINT ( 'NONE',  ( 1.415196051561583790, -4.795541693661363958, -5.250000000000000888 ) ) ;
#3283 = FACE_BOUND ( 'NONE', #12989, .T. ) ;
#3282 = AXIS2_PLACEMENT_3D ( 'NONE', #11517, #7666, #12565 ) ;
#3284 = DIRECTION ( 'NONE',  ( -0.000000000000000000, -1.000000000000000000, -0.000000000000000000 ) ) ;
#3285 = DIRECTION ( 'NONE',  ( 0.000000000000000000, 1.000000000000000000, 0.000000000000000000 ) ) ;
#3286 = DIRECTION ( 'NONE',  ( -0.000000000000000000, -1.000000000000000000, -0.000000000000000000 ) ) ;
#3287 = CARTESIAN_POINT ( 'NONE',  ( -5.000000000000000888, 6.123233995736767268E-16, -25.03750572909317285 ) ) ;
#3288 = CARTESIAN_POINT ( 'NONE',  ( 1.846868145590736310, -29.87500000136559564, 4.458734124999997661 ) ) ;
#3289 = CARTESIAN_POINT ( 'NONE',  ( -1.261996585732579224, 4.276409079477648589, -0.06249999863440838799 ) ) ;
#3290 = ORIENTED_EDGE ( 'NONE', *, *, #9991, .F. ) ;
#3291 = DIRECTION ( 'NONE',  ( -0.000000000000000000, 1.000000000000000000, -0.000000000000000000 ) ) ;
#3292 = EDGE_LOOP ( 'NONE', ( #5754, #2584, #1112, #4327, #5277 ) ) ;
#3293 = ORIENTED_EDGE ( 'NONE', *, *, #11906, .F. ) ;
#3294 =( NAMED_UNIT ( * ) PLANE_ANGLE_UNIT ( ) SI_UNIT ( $, .RADIAN. ) );
#3295 = CARTESIAN_POINT ( 'NONE',  ( -4.458734124999999437, -28.18750000136559564, -5.460374474430324690E-16 ) ) ;
#3296 = CARTESIAN_POINT ( 'NONE',  ( 0.5711823568785988625, 5.381735091635026613, -7.812500000000005329 ) ) ;
#3297 = CIRCLE ( 'NONE', #15434, 5.000000000000000000 ) ;
#3298 = EDGE_CURVE ( 'NONE', #1232, #12621, #8311, .T. ) ;
#3299 = DIRECTION ( 'NONE',  ( 0.000000000000000000, 0.000000000000000000, 1.000000000000000000 ) ) ;
#3300 = DIRECTION ( 'NONE',  ( 0.000000000000000000, 0.000000000000000000, 1.000000000000000000 ) ) ;
#3301 = CARTESIAN_POINT ( 'NONE',  ( 2.131511515620586383, 3.916244202832140253, -7.187499998634407916 ) ) ;
#3302 = CARTESIAN_POINT ( 'NONE',  ( 3.093157300003885890, 6.874418838041284729, 2.320870275476782535E-15 ) ) ;
#3303 = CARTESIAN_POINT ( 'NONE',  ( -3.535533905932737309, -26.62500000000000000, -3.535533905932738197 ) ) ;
#3304 = CARTESIAN_POINT ( 'NONE',  ( -4.209348295687703967, -3.401574460001763001, 1.562499999999996669 ) ) ;
#3305 = DIRECTION ( 'NONE',  ( 0.4999999999999973355, 0.8660254037844402619, -0.000000000000000000 ) ) ;
#3306 = CIRCLE ( 'NONE', #7443, 2.500000000000001332 ) ;
#3307 = EDGE_CURVE ( 'NONE', #11884, #2379, #14118, .T. ) ;
#3308 = DIRECTION ( 'NONE',  ( 0.000000000000000000, 0.000000000000000000, 1.000000000000000000 ) ) ;
#3309 = CARTESIAN_POINT ( 'NONE',  ( 2.071067811865475505, -21.93750000273119127, -5.000000000000000888 ) ) ;
#3310 = ORIENTED_EDGE ( 'NONE', *, *, #2500, .F. ) ;
#3311 = CARTESIAN_POINT ( 'NONE',  ( 1.846868145590735200, -22.25000000136559564, -4.458734124999999437 ) ) ;
#3312 =( REPRESENTATION_RELATIONSHIP ('NONE','NONE', #4176, #6981 ) REPRESENTATION_RELATIONSHIP_WITH_TRANSFORMATION ( #15128 )SHAPE_REPRESENTATION_RELATIONSHIP( ) );
#3313 = EDGE_CURVE ( 'NONE', #7552, #12557, #9577, .T. ) ;
#3314 = CARTESIAN_POINT ( 'NONE',  ( 0.000000000000000000, 40.00000000000000000, 0.000000000000000000 ) ) ;
#3315 = ORIENTED_EDGE ( 'NONE', *, *, #6324, .T. ) ;
#3316 = ORIENTED_EDGE ( 'NONE', *, *, #2335, .F. ) ;
#3317 = CARTESIAN_POINT ( 'NONE',  ( -4.391654775818395251, 2.390265326283148806, -3.499999997268816276 ) ) ;
#3318 = AXIS2_PLACEMENT_3D ( 'NONE', #6996, #10701, #8296 ) ;
#3319 = CARTESIAN_POINT ( 'NONE',  ( 4.458734125000000326, -29.37500000136559208, -1.846868145590734978 ) ) ;
#3320 = CYLINDRICAL_SURFACE ( 'NONE', #14860, 5.000000000000000000 ) ;
#3321 = EDGE_LOOP ( 'NONE', ( #11251, #11938, #8241, #4990 ) ) ;
#3322 = DIRECTION ( 'NONE',  ( -1.000000000000000000, 0.000000000000000000, 0.000000000000000000 ) ) ;
#3323 = STYLED_ITEM ( 'NONE', ( #14492 ), #9475 ) ;
#3324 = DIRECTION ( 'NONE',  ( 0.000000000000000000, 1.000000000000000000, 0.000000000000000000 ) ) ;
#3325 = CARTESIAN_POINT ( 'NONE',  ( 3.152801135295367541, -27.56250000136559564, -3.152801135295367541 ) ) ;
#3326 = CIRCLE ( 'NONE', #7213, 2.500000000000001332 ) ;
#3327 = EDGE_CURVE ( 'NONE', #379, #2190, #12096, .T. ) ;
#3328 = CARTESIAN_POINT ( 'NONE',  ( -19.99999999999956657, -20.00000000000000000, -2.499999999999120259 ) ) ;
#3329 = DIRECTION ( 'NONE',  ( 0.000000000000000000, 0.000000000000000000, 1.000000000000000000 ) ) ;
#3330 = SURFACE_SIDE_STYLE ('',( #15617 ) ) ;
#3331 = CARTESIAN_POINT ( 'NONE',  ( -91.33974596215558961, -110.0591436588189254, 17.50000000000000000 ) ) ;
#3332 = ADVANCED_FACE ( 'NONE', ( #7249 ), #12072, .F. ) ;
#3334 = EDGE_CURVE ( 'NONE', #13329, #1672, #1016, .T. ) ;
#3333 = EDGE_LOOP ( 'NONE', ( #12994, #325 ) ) ;
#3335 = AXIS2_PLACEMENT_3D ( 'NONE', #5488, #14219, #2893 ) ;
#3336 = ORIENTED_EDGE ( 'NONE', *, *, #1140, .F. ) ;
#3337 = CARTESIAN_POINT ( 'NONE',  ( -4.000000000000000000, 0.7924765000094600165, -0.05906175389889745803 ) ) ;
#3338 = ORIENTED_EDGE ( 'NONE', *, *, #4488, .T. ) ;
#3339 = CARTESIAN_POINT ( 'NONE',  ( 35.00000000000000000, 40.00000000000000000, -8.572527594031472993E-15 ) ) ;
#3340 = FACE_OUTER_BOUND ( 'NONE', #2359, .T. ) ;
#3341 = CARTESIAN_POINT ( 'NONE',  ( -0.5093500532425060401, -4.799145180956616130, 1.375000001365592528 ) ) ;
#3342 = DIRECTION ( 'NONE',  ( -0.8660254037844364872, 0.000000000000000000, -0.5000000000000041078 ) ) ;
#3343 = CARTESIAN_POINT ( 'NONE',  ( 3.753672977998667726, 3.033343224707664376, -3.499999998634410137 ) ) ;
#3344 = LINE ( 'NONE', #8208, #12889 ) ;
#3345 = CARTESIAN_POINT ( 'NONE',  ( 5.000000000000000000, -22.18750000273118772, 2.071067811865478614 ) ) ;
#3346 = EDGE_CURVE ( 'NONE', #7037, #1654, #14509, .T. ) ;
#3347 = EDGE_LOOP ( 'NONE', ( #5791, #8130, #7271, #13989 ) ) ;
#3348 = DIRECTION ( 'NONE',  ( 0.000000000000000000, 1.000000000000000000, 0.000000000000000000 ) ) ;
#3349 = CARTESIAN_POINT ( 'NONE',  ( -113.6871902368263250, -110.1917077999037957, 17.50000000000000000 ) ) ;
#3350 = B_SPLINE_CURVE_WITH_KNOTS ( 'NONE', 3,
 ( #2048, #4792, #12131, #2357, #3488, #998, #4635, #5932 ),
 .UNSPECIFIED., .F., .F.,
 ( 4, 2, 2, 4 ),
 ( 7.780516681398759253E-20, 0.002450665683189819696, 0.003675998524784729327, 0.004901331366379639391 ),
 .UNSPECIFIED. ) ;
#3351 = VERTEX_POINT ( 'NONE', #3505 ) ;
#3352 = DIRECTION ( 'NONE',  ( 0.000000000000000000, 0.000000000000000000, 1.000000000000000000 ) ) ;
#3353 = EDGE_LOOP ( 'NONE', ( #1617, #12654, #419, #8201 ) ) ;
#3354 = ORIENTED_EDGE ( 'NONE', *, *, #13324, .F. ) ;
#3355 = CARTESIAN_POINT ( 'NONE',  ( -3.753672977998669502, -3.033343224707661712, -0.9999999986344076941 ) ) ;
#3356 = CARTESIAN_POINT ( 'NONE',  ( 24.26932219902320043, 20.00000000000000000, -5.999999999999989342 ) ) ;
#3357 = FACE_OUTER_BOUND ( 'NONE', #6836, .T. ) ;
#3358 = DIRECTION ( 'NONE',  ( -1.000000000000000000, -0.000000000000000000, -0.000000000000000000 ) ) ;
#3359 = CARTESIAN_POINT ( 'NONE',  ( 2.500000000000000000, 2.357898499370433054, -1.951563910473907981E-15 ) ) ;
#3360 = CARTESIAN_POINT ( 'NONE',  ( 0.000000000000000000, 0.000000000000000000, -25.03750572909317285 ) ) ;
#3361 = DIRECTION ( 'NONE',  ( 0.000000000000000000, 0.000000000000000000, -1.000000000000000000 ) ) ;
#3362 = EDGE_CURVE ( 'NONE', #14429, #395, #15202, .T. ) ;
#3363 = DIRECTION ( 'NONE',  ( 1.000000000000000000, 0.000000000000000000, 0.000000000000000000 ) ) ;
#3364 = ADVANCED_FACE ( 'NONE', ( #1323 ), #9892, .T. ) ;
#3365 = CARTESIAN_POINT ( 'NONE',  ( 3.152801135295366208, -30.81250000136559564, 3.152801135295367985 ) ) ;
#3366 = EDGE_CURVE ( 'NONE', #362, #1764, #13893, .T. ) ;
#3367 = CARTESIAN_POINT ( 'NONE',  ( -4.276409079477644148, -1.261996585732578335, -1.812499998634406584 ) ) ;
#3368 = VERTEX_POINT ( 'NONE', #3431 ) ;
#3369 = CARTESIAN_POINT ( 'NONE',  ( 0.3306966981844952636, 8.469326210127450238, -7.349897473154610950 ) ) ;
#3370 = EDGE_LOOP ( 'NONE', ( #12716, #13421, #1272, #11790, #2582 ) ) ;
#3371 = VERTEX_POINT ( 'NONE', #9650 ) ;
#3372 = ORIENTED_EDGE ( 'NONE', *, *, #1820, .T. ) ;
#3373 = CARTESIAN_POINT ( 'NONE',  ( 1.846868145590736310, -25.87500000136559919, 4.458734124999999437 ) ) ;
#3374 = CARTESIAN_POINT ( 'NONE',  ( 0.000000000000000000, -20.00000000000000000, 0.000000000000000000 ) ) ;
#3375 = FACE_OUTER_BOUND ( 'NONE', #13788, .T. ) ;
#3376 = CARTESIAN_POINT ( 'NONE',  ( 2.452879891156804160, 7.244083172395184178, -0.1007566405101766455 ) ) ;
#3377 = DIRECTION ( 'NONE',  ( 1.000000000000000000, 0.000000000000000000, 0.000000000000000000 ) ) ;
#3378 = CARTESIAN_POINT ( 'NONE',  ( 2.131511515620586383, 3.916244202832140253, -6.187499998634407028 ) ) ;
#3379 = CARTESIAN_POINT ( 'NONE',  ( 39.53738644056087992, -3.000000000000000000, -28.48076211352192999 ) ) ;
#3380 = CARTESIAN_POINT ( 'NONE',  ( -1.344377895606795770, -4.647603660250892332, -0.1184410768129991742 ) ) ;
#3381 = CARTESIAN_POINT ( 'NONE',  ( -9.184850993605147944E-16, -21.37500000273118772, 5.000000000000000000 ) ) ;
#3382 = EDGE_CURVE ( 'NONE', #5667, #6319, #9012, .T. ) ;
#3383 = ORIENTED_EDGE ( 'NONE', *, *, #9107, .T. ) ;
#3384 = DIRECTION ( 'NONE',  ( 0.000000000000000000, 0.000000000000000000, 1.000000000000000000 ) ) ;
#3385 = ORIENTED_EDGE ( 'NONE', *, *, #585, .T. ) ;
#3386 = MANIFOLD_SOLID_BREP ( 'Fillet1', #2750 ) ;
#3387 = VERTEX_POINT ( 'NONE', #4892 ) ;
#3388 = PLANE ( 'NONE',  #6702 ) ;
#3389 = CARTESIAN_POINT ( 'NONE',  ( 3.152801135295367541, -29.31250000136559208, -3.152801135295367541 ) ) ;
#3390 = CARTESIAN_POINT ( 'NONE',  ( 19.99999999999956657, -8.786575603324269439E-13, 1.500000000000000000 ) ) ;
#3391 = ORIENTED_EDGE ( 'NONE', *, *, #83, .T. ) ;
#3392 = CARTESIAN_POINT ( 'NONE',  ( 0.000000000000000000, 0.000000000000000000, 0.000000000000000000 ) ) ;
#3393 = CARTESIAN_POINT ( 'NONE',  ( -1.211595439868048407, 7.960739084487649109, -0.4504974108211993733 ) ) ;
#3394 = CARTESIAN_POINT ( 'NONE',  ( 40.79999760747214310, -3.012271619929379973, -27.17815842419070194 ) ) ;
#3395 = CARTESIAN_POINT ( 'NONE',  ( 2.730187237215162345E-16, -23.43750000136559564, -4.458734124999999437 ) ) ;
#3396 = CARTESIAN_POINT ( 'NONE',  ( 10.00000000000098765, -13.00000000000000178, 17.32050807568871065 ) ) ;
#3397 = CARTESIAN_POINT ( 'NONE',  ( -4.209348295687703079, -3.401574460001763445, -0.3124999972688167760 ) ) ;
#3398 = B_SPLINE_CURVE_WITH_KNOTS ( 'NONE', 3,
 ( #7716, #8763, #11166, #7793 ),
 .UNSPECIFIED., .F., .F.,
 ( 4, 4 ),
 ( 0.000000000000000000, 0.002452478801916361129 ),
 .UNSPECIFIED. ) ;
#3399 = FACE_OUTER_BOUND ( 'NONE', #15186, .T. ) ;
#3400 = AXIS2_PLACEMENT_3D ( 'NONE', #2340, #5091, #14962 ) ;
#3401 = VERTEX_POINT ( 'NONE', #1246 ) ;
#3402 = FILL_AREA_STYLE ('',( #595 ) ) ;
#3403 = VERTEX_POINT ( 'NONE', #6194 ) ;
#3404 = CARTESIAN_POINT ( 'NONE',  ( -0.9763930676191269198, 8.096533237419631490, -7.213065638944388347 ) ) ;
#3405 = VERTEX_POINT ( 'NONE', #11347 ) ;
#3406 = CARTESIAN_POINT ( 'NONE',  ( 0.000000000000000000, 0.000000000000000000, 0.000000000000000000 ) ) ;
#3407 = EDGE_CURVE ( 'NONE', #8136, #14464, #7485, .T. ) ;
#3408 = CARTESIAN_POINT ( 'NONE',  ( -24.26932219902320043, 20.00000000000000000, -5.999999999999984901 ) ) ;
#3409 = CARTESIAN_POINT ( 'NONE',  ( -3.916244202832140253, 2.131511515620587272, -0.9374999986344056957 ) ) ;
#3410 = CARTESIAN_POINT ( 'NONE',  ( 42.02221399786069611, -8.000000000000003553, 1.040834085586084257E-13 ) ) ;
#3411 = CARTESIAN_POINT ( 'NONE',  ( -2.131511515620587272, -3.916244202832140253, -1.937499998634406584 ) ) ;
#3412 = CARTESIAN_POINT ( 'NONE',  ( 0.000000000000000000, 37.00000000000000000, 0.000000000000000000 ) ) ;
#3413 = DIRECTION ( 'NONE',  ( -0.000000000000000000, -1.000000000000000000, -0.000000000000000000 ) ) ;
#3414 = ORIENTED_EDGE ( 'NONE', *, *, #15028, .T. ) ;
#3415 = DIRECTION ( 'NONE',  ( -1.000000000000000000, 0.000000000000000000, -3.343241100358131282E-16 ) ) ;
#3416 = DIRECTION ( 'NONE',  ( 1.000000000000000000, 0.000000000000000000, 0.000000000000000000 ) ) ;
#3417 = ORIENTED_EDGE ( 'NONE', *, *, #15234, .T. ) ;
#3418 = DIRECTION ( 'NONE',  ( 0.000000000000000000, 0.000000000000000000, -1.000000000000000000 ) ) ;
#3419 = VERTEX_POINT ( 'NONE', #13682 ) ;
#3420 = VECTOR ( 'NONE', #3324, 1000.000000000000000 ) ;
#3421 = ORIENTED_EDGE ( 'NONE', *, *, #10047, .T. ) ;
#3422 = CARTESIAN_POINT ( 'NONE',  ( 4.276409079477644148, 1.261996585732577891, -2.562499998634407028 ) ) ;
#3423 = AXIS2_PLACEMENT_3D ( 'NONE', #12803, #5548, #1899 ) ;
#3424 = CARTESIAN_POINT ( 'NONE',  ( -60.00000000000000000, -37.00000000000000711, -20.00000000000000711 ) ) ;
#3425 = EDGE_CURVE ( 'NONE', #9981, #757, #15430, .T. ) ;
#3426 = EDGE_CURVE ( 'NONE', #4597, #4915, #11486, .T. ) ;
#3427 = DIRECTION ( 'NONE',  ( -1.000000000000000000, 0.000000000000000000, 0.000000000000000000 ) ) ;
#3428 = DIRECTION ( 'NONE',  ( 0.000000000000000000, 1.000000000000000000, 0.000000000000000000 ) ) ;
#3429 = CARTESIAN_POINT ( 'NONE',  ( 0.000000000000000000, 40.00000000000000000, -57.99999999999999289 ) ) ;
#3430 = CARTESIAN_POINT ( 'NONE',  ( 8.152940247294426498E-14, -9.016621985895911351, -7.999704684617491068 ) ) ;
#3431 = CARTESIAN_POINT ( 'NONE',  ( -9.184850993605147944E-16, -30.25000000000000000, 5.000000000000000000 ) ) ;
#3432 = CARTESIAN_POINT ( 'NONE',  ( -4.458734124999999437, -30.25000000136559919, -1.846868145590735644 ) ) ;
#3433 = CARTESIAN_POINT ( 'NONE',  ( -3.916244202832140253, 2.131511515620587272, 1.062500001365592528 ) ) ;
#3434 = ORIENTED_EDGE ( 'NONE', *, *, #3164, .T. ) ;
#3435 = CARTESIAN_POINT ( 'NONE',  ( 0.000000000000000000, 50.00000000000000000, 0.000000000000000000 ) ) ;
#3436 = ORIENTED_EDGE ( 'NONE', *, *, #3346, .T. ) ;
#3437 = ORIENTED_EDGE ( 'NONE', *, *, #8142, .T. ) ;
#3438 = ORIENTED_EDGE ( 'NONE', *, *, #6306, .F. ) ;
#3439 = PRODUCT_DEFINITION_SHAPE ( 'NONE', 'NONE',  #15967 ) ;
#3440 = CARTESIAN_POINT ( 'NONE',  ( -3.152801135295367985, -26.06250000136559919, 3.152801135295367096 ) ) ;
#3441 = LINE ( 'NONE', #8394, #9959 ) ;
#3442 = FACE_OUTER_BOUND ( 'NONE', #11276, .T. ) ;
#3443 = EDGE_CURVE ( 'NONE', #1108, #11572, #14901, .T. ) ;
#3444 = AXIS2_PLACEMENT_3D ( 'NONE', #612, #1805, #5612 ) ;
#3445 = EDGE_CURVE ( 'NONE', #6536, #9071, #1644, .T. ) ;
#3446 = FACE_OUTER_BOUND ( 'NONE', #1170, .T. ) ;
#3447 = CARTESIAN_POINT ( 'NONE',  ( 0.000000000000000000, 0.000000000000000000, -8.499999999999996447 ) ) ;
#3448 = CARTESIAN_POINT ( 'NONE',  ( -2.071067811865478170, -23.31249999999999645, 5.000000000000000000 ) ) ;
#3449 = CARTESIAN_POINT ( 'NONE',  ( -4.795541693661363958, -1.415196051561583790, -1.500000000000001332 ) ) ;
#3450 = DIRECTION ( 'NONE',  ( 0.000000000000000000, -0.000000000000000000, 1.000000000000000000 ) ) ;
#3451 = CARTESIAN_POINT ( 'NONE',  ( -9.184850993605147944E-16, -27.25000000000000000, 5.000000000000000000 ) ) ;
#3452 = CARTESIAN_POINT ( 'NONE',  ( -8.190561711645485556E-16, -30.68750000136559564, 4.458734124999999437 ) ) ;
#3453 = EDGE_LOOP ( 'NONE', ( #1135, #15407 ) ) ;
#3454 = DIRECTION ( 'NONE',  ( 0.8660254037844405950, -0.4999999999999965028, -0.000000000000000000 ) ) ;
#3455 = VERTEX_POINT ( 'NONE', #216 ) ;
#3456 = EDGE_LOOP ( 'NONE', ( #2394, #3186 ) ) ;
#3457 = CARTESIAN_POINT ( 'NONE',  ( -7.500000000000003553, 1.644753667985980217, -7.029983668656051066 ) ) ;
#3458 = MECHANICAL_DESIGN_GEOMETRIC_PRESENTATION_REPRESENTATION (  '', ( #114 ), #10179 ) ;
#3459 = CARTESIAN_POINT ( 'NONE',  ( 4.458734124999999437, -27.50000000136559208, 1.846868145590737864 ) ) ;
#3460 = CYLINDRICAL_SURFACE ( 'NONE', #9949, 2.500000000000000888 ) ;
#3461 = AXIS2_PLACEMENT_3D ( 'NONE', #12185, #1287, #1124 ) ;
#3462 = ORIENTED_EDGE ( 'NONE', *, *, #4479, .T. ) ;
#3463 = DIRECTION ( 'NONE',  ( -0.000000000000000000, 1.000000000000000000, -0.000000000000000000 ) ) ;
#3464 = ADVANCED_FACE ( 'NONE', ( #4071 ), #11500, .T. ) ;
#3465 = CARTESIAN_POINT ( 'NONE',  ( 42.02221399786069611, 0.000000000000000000, -2.649999999999884892 ) ) ;
#3466 = FACE_OUTER_BOUND ( 'NONE', #9360, .T. ) ;
#3467 = CARTESIAN_POINT ( 'NONE',  ( -21.01110699893060030, 0.000000000000000000, 36.39230484541324273 ) ) ;
#3468 = CARTESIAN_POINT ( 'NONE',  ( 3.152801135295367541, -23.56250000136559564, -3.152801135295367541 ) ) ;
#3469 = DIRECTION ( 'NONE',  ( -1.000000000000000000, -0.000000000000000000, -0.000000000000000000 ) ) ;
#3470 = CARTESIAN_POINT ( 'NONE',  ( -21.01110699893041911, 0.000000000000000000, -39.04230484541333368 ) ) ;
#3471 =( NAMED_UNIT ( * ) PLANE_ANGLE_UNIT ( ) SI_UNIT ( $, .RADIAN. ) );
#3472 = CIRCLE ( 'NONE', #10961, 75.00000000000004263 ) ;
#3473 = CARTESIAN_POINT ( 'NONE',  ( 4.211140560182196957, -2.431303136016555122, -3.745885042887436622 ) ) ;
#3474 = EDGE_LOOP ( 'NONE', ( #14614, #12377, #2125, #4222, #11847, #9762, #6762, #14706, #14265 ) ) ;
#3475 = SHAPE_REPRESENTATION_RELATIONSHIP ( 'NONE' , 'NONE' ,  #3173, #15834 ) ;
#3476 = VERTEX_POINT ( 'NONE', #12629 ) ;
#3477 = CARTESIAN_POINT ( 'NONE',  ( -91.33974596215551855, -10.00000000000002487, -17.50000000000000000 ) ) ;
#3478 = CIRCLE ( 'NONE', #2964, 2.500000000000000444 ) ;
#3479 = ORIENTED_EDGE ( 'NONE', *, *, #9313, .T. ) ;
#3480 = EDGE_CURVE ( 'NONE', #11871, #12864, #13849, .T. ) ;
#3481 = CARTESIAN_POINT ( 'NONE',  ( 0.000000000000000000, -20.00000000000000000, -25.00000000000000000 ) ) ;
#3482 = CYLINDRICAL_SURFACE ( 'NONE', #7462, 2.649999999999992806 ) ;
#3483 = CARTESIAN_POINT ( 'NONE',  ( 5.000000000000000888, -27.93750000000000711, -2.071067811865475505 ) ) ;
#3484 = DIRECTION ( 'NONE',  ( 1.000000000000000000, -6.123233995736766036E-17, -6.123233995736764803E-17 ) ) ;
#3485 = CIRCLE ( 'NONE', #9438, 40.00000000000001421 ) ;
#3486 = CARTESIAN_POINT ( 'NONE',  ( 4.276409079477644148, 1.261996585732577891, -0.5624999986344088043 ) ) ;
#3487 = SURFACE_SIDE_STYLE ('',( #15953 ) ) ;
#3488 = CARTESIAN_POINT ( 'NONE',  ( 2.804994570502171047, 3.229033611042449792, -3.526374918436834704 ) ) ;
#3489 = VERTEX_POINT ( 'NONE', #2779 ) ;
#3490 = LINE ( 'NONE', #4713, #2019 ) ;
#3491 = SURFACE_SIDE_STYLE ('',( #2432 ) ) ;
#3492 = EDGE_CURVE ( 'NONE', #10008, #5750, #2669, .T. ) ;
#3493 = ORIENTED_EDGE ( 'NONE', *, *, #13493, .T. ) ;
#3494 = CARTESIAN_POINT ( 'NONE',  ( 4.999999999999849898, -1.272547481429010530, -1.086597482644648061 ) ) ;
#3495 = ORIENTED_EDGE ( 'NONE', *, *, #7519, .T. ) ;
#3496 = ORIENTED_EDGE ( 'NONE', *, *, #10229, .F. ) ;
#3497 = CARTESIAN_POINT ( 'NONE',  ( 1.261996585732578113, -4.276409079477644148, -2.812499998634407472 ) ) ;
#3498 = VECTOR ( 'NONE', #4013, 1000.000000000000000 ) ;
#3499 = DIRECTION ( 'NONE',  ( 0.000000000000000000, 0.000000000000000000, 1.000000000000000000 ) ) ;
#3500 = AXIS2_PLACEMENT_3D ( 'NONE', #5960, #2151, #8629 ) ;
#3501 = CARTESIAN_POINT ( 'NONE',  ( 19.99999999999956657, -8.786575603324269439E-13, -11.50000000000000000 ) ) ;
#3502 = DIRECTION ( 'NONE',  ( 0.5000000000000005551, 0.000000000000000000, -0.8660254037844382635 ) ) ;
#3503 = CARTESIAN_POINT ( 'NONE',  ( 4.211140560182196957, 2.431303136016536470, -3.745885042887433514 ) ) ;
#3504 = CARTESIAN_POINT ( 'NONE',  ( -4.391654775818395251, 2.390265326283148806, -1.499999997268814500 ) ) ;
#3505 = CARTESIAN_POINT ( 'NONE',  ( -7.500000000000000888, -4.330127018922199866, -1.000000000000000888 ) ) ;
#3506 = STYLED_ITEM ( 'NONE', ( #6085 ), #3780 ) ;
#3507 = CARTESIAN_POINT ( 'NONE',  ( -4.618802153516977427, -3.000000000000000000, -36.00000000000000711 ) ) ;
#3508 = CARTESIAN_POINT ( 'NONE',  ( 2.730187237215162345E-16, -27.43750000136559564, -4.458734124999999437 ) ) ;
#3509 = CARTESIAN_POINT ( 'NONE',  ( 0.5093500532425063732, 4.799145180956616130, -6.124999998634407916 ) ) ;
#3510 = VERTEX_POINT ( 'NONE', #2931 ) ;
#3511 = DIRECTION ( 'NONE',  ( -0.000000000000000000, -1.000000000000000000, -0.000000000000000000 ) ) ;
#3512 = EDGE_CURVE ( 'NONE', #4240, #10129, #2439, .T. ) ;
#3513 = EDGE_LOOP ( 'NONE', ( #7034, #12791, #2347 ) ) ;
#3514 = EDGE_LOOP ( 'NONE', ( #2034, #4762, #7178, #15022 ) ) ;
#3515 = EDGE_CURVE ( 'NONE', #15896, #5616, #5137, .T. ) ;
#3516 = VECTOR ( 'NONE', #9867, 1000.000000000000000 ) ;
#3517 = ORIENTED_EDGE ( 'NONE', *, *, #12522, .T. ) ;
#3518 = AXIS2_PLACEMENT_3D ( 'NONE', #7554, #14986, #4060 ) ;
#3519 = CARTESIAN_POINT ( 'NONE',  ( 2.730187237215162345E-16, -23.43750000136559564, -4.458734124999999437 ) ) ;
#3520 = CARTESIAN_POINT ( 'NONE',  ( 24.26932219902320043, 37.00000000000000000, -5.999999999999989342 ) ) ;
#3521 = CARTESIAN_POINT ( 'NONE',  ( 3.535533905932736864, -30.25000000273118417, 3.535533905932738641 ) ) ;
#3522 = CIRCLE ( 'NONE', #2753, 2.500000000000909495 ) ;
#3523 = DIRECTION ( 'NONE',  ( -0.000000000000000000, -0.000000000000000000, -1.000000000000000000 ) ) ;
#3524 = DIRECTION ( 'NONE',  ( 0.000000000000000000, 1.000000000000000000, 0.000000000000000000 ) ) ;
#3525 = CARTESIAN_POINT ( 'NONE',  ( 5.000000000000000888, -23.93750000000000000, -2.071067811865475505 ) ) ;
#3526 = CARTESIAN_POINT ( 'NONE',  ( 5.000000000000000000, -23.00000000000000000, 0.000000000000000000 ) ) ;
#3527 = VECTOR ( 'NONE', #1635, 1000.000000000000000 ) ;
#3528 = CARTESIAN_POINT ( 'NONE',  ( 0.5711823568785989735, 5.381735091635026613, -2.812500000000001332 ) ) ;
#3529 = CARTESIAN_POINT ( 'NONE',  ( -2.499999999999999556, 3.061616997868382648E-16, 3.469446951953614189E-15 ) ) ;
#3530 = CARTESIAN_POINT ( 'NONE',  ( 3.061616997868383141E-16, -29.75000000000000000, -5.000000000000000000 ) ) ;
#3531 = CARTESIAN_POINT ( 'NONE',  ( 4.458734125000000326, -31.37500000136559564, -1.846868145590734978 ) ) ;
#3532 = CARTESIAN_POINT ( 'NONE',  ( -3.753672977998669946, -3.033343224707661712, -1.999999998634408360 ) ) ;
#3533 = ORIENTED_EDGE ( 'NONE', *, *, #5671, .T. ) ;
#3534 = CARTESIAN_POINT ( 'NONE',  ( -39.99999999999999289, -13.00000000000000178, -2.500000000000079492 ) ) ;
#3535 = ORIENTED_EDGE ( 'NONE', *, *, #12820, .T. ) ;
#3536 = ORIENTED_EDGE ( 'NONE', *, *, #521, .T. ) ;
#3537 = ADVANCED_FACE ( 'NONE', ( #9977 ), #14916, .F. ) ;
#3538 = CARTESIAN_POINT ( 'NONE',  ( 35.00000000000000000, 37.00000000000000000, 5.999999999999991118 ) ) ;
#3539 = CARTESIAN_POINT ( 'NONE',  ( 3.152801135295366208, -24.56250000136559564, 3.152801135295367985 ) ) ;
#3540 = DIRECTION ( 'NONE',  ( 0.8306121863236411995, 0.2451191463975535001, -0.4999999999999953371 ) ) ;
#3541 = VERTEX_POINT ( 'NONE', #14997 ) ;
#3542 = AXIS2_PLACEMENT_3D ( 'NONE', #11503, #374, #7890 ) ;
#3543 = CARTESIAN_POINT ( 'NONE',  ( -67.50000000000000000, 50.00000000000000000, 2.649999999999285816 ) ) ;
#3545 = VECTOR ( 'NONE', #2823, 1000.000000000000000 ) ;
#3544 = PLANE ( 'NONE',  #4876 ) ;
#3546 = CARTESIAN_POINT ( 'NONE',  ( -1.312671235360383548, -3.860931062424228788, -0.05923475698271369466 ) ) ;
#3547 = DIRECTION ( 'NONE',  ( 1.000000000000000000, 0.000000000000000000, 0.000000000000000000 ) ) ;
#3548 = AXIS2_PLACEMENT_3D ( 'NONE', #10049, #6414, #2673 ) ;
#3549 = CARTESIAN_POINT ( 'NONE',  ( 1.846868145590736310, -21.87500000136559208, 4.458734124999999437 ) ) ;
#3550 = FACE_OUTER_BOUND ( 'NONE', #12172, .T. ) ;
#3551 = DIRECTION ( 'NONE',  ( 0.000000000000000000, 0.000000000000000000, 1.000000000000000000 ) ) ;
#3552 = CARTESIAN_POINT ( 'NONE',  ( -5.000000000000000000, -30.62500000273118772, -6.123233995736766282E-16 ) ) ;
#3553 = LINE ( 'NONE', #8513, #5240 ) ;
#3554 = CIRCLE ( 'NONE', #13882, 3.499999999999999556 ) ;
#3555 = CARTESIAN_POINT ( 'NONE',  ( 25.00000000000000000, 2.516649172247811061E-16, -2.055000000000000160 ) ) ;
#3556 = EDGE_CURVE ( 'NONE', #9570, #14100, #11185, .T. ) ;
#3557 = CARTESIAN_POINT ( 'NONE',  ( 5.000000000000000000, -25.00000000000000000, 0.000000000000000000 ) ) ;
#3559 = EDGE_CURVE ( 'NONE', #6711, #2479, #1376, .T. ) ;
#3558 = ORIENTED_EDGE ( 'NONE', *, *, #9039, .T. ) ;
#3560 = EDGE_CURVE ( 'NONE', #715, #7857, #10432, .T. ) ;
#3561 =( BOUNDED_CURVE ( )  B_SPLINE_CURVE ( 2, ( #962, #13450, #69, #12094, #15831, #6045, #11058, #2322, #3451 ),
 .UNSPECIFIED., .F., .F. ) 
 B_SPLINE_CURVE_WITH_KNOTS ( ( 3, 2, 2, 2, 3 ),
 ( 0.4250000000000000444, 0.4375000000000000555, 0.4500000000000000666, 0.4625000000000001332, 0.4750000000000000888 ),
 .UNSPECIFIED. ) 
 CURVE ( )  GEOMETRIC_REPRESENTATION_ITEM ( )  RATIONAL_B_SPLINE_CURVE ( ( 0.9999999999999996669, 0.9238795325112870716, 1.000000000000000000, 0.9238795325112867385, 1.000000000000000000, 0.9238795325112867385, 1.000000000000000000, 0.9238795325112860723, 1.000000000000000666 ) ) 
 REPRESENTATION_ITEM ( '' )  );
#3562 = EDGE_CURVE ( 'NONE', #8889, #3476, #6992, .T. ) ;
#3563 = AXIS2_PLACEMENT_3D ( 'NONE', #10513, #8093, #4438 ) ;
#3564 = ORIENTED_EDGE ( 'NONE', *, *, #6146, .T. ) ;
#3565 = DIRECTION ( 'NONE',  ( -0.000000000000000000, 1.000000000000000000, -0.000000000000000000 ) ) ;
#3566 = AXIS2_PLACEMENT_3D ( 'NONE', #840, #10853, #11969 ) ;
#3567 = ORIENTED_EDGE ( 'NONE', *, *, #12620, .F. ) ;
#3568 = CIRCLE ( 'NONE', #10559, 0.7733184030943203169 ) ;
#3569 = DIRECTION ( 'NONE',  ( 0.000000000000000000, 0.000000000000000000, 1.000000000000000000 ) ) ;
#3570 = CARTESIAN_POINT ( 'NONE',  ( 39.73786839672636262, -3.982459619754358027, 28.28175983491992440 ) ) ;
#3571 = CARTESIAN_POINT ( 'NONE',  ( -1.261996585732579224, 4.276409079477648589, -0.06249999863440838799 ) ) ;
#3572 = AXIS2_PLACEMENT_3D ( 'NONE', #15699, #10763, #2105 ) ;
#3573 = CARTESIAN_POINT ( 'NONE',  ( -67.50000000000000000, 32.00000000000000000, -7.070249711157346244E-13 ) ) ;
#3574 = VECTOR ( 'NONE', #7844, 1000.000000000000114 ) ;
#3575 = PRODUCT ( 'Circular Main Body Shell', 'Circular Main Body Shell', '', ( #1792 ) ) ;
#3576 = CARTESIAN_POINT ( 'NONE',  ( -4.276409079477644148, -1.261996585732578335, -3.062499998634407472 ) ) ;
#3577 = FACE_OUTER_BOUND ( 'NONE', #13494, .T. ) ;
#3578 = LINE ( 'NONE', #7381, #5890 ) ;
#3579 = EDGE_LOOP ( 'NONE', ( #10493, #4203, #6813, #9254 ) ) ;
#3580 = CARTESIAN_POINT ( 'NONE',  ( -6.765421556309547668E-13, 50.00000000000000000, 70.14999999999929514 ) ) ;
#3581 = EDGE_CURVE ( 'NONE', #11709, #621, #11584, .T. ) ;
#3582 = CIRCLE ( 'NONE', #5660, 4.250000000000000000 ) ;
#3583 =( NAMED_UNIT ( * ) SI_UNIT ( $, .STERADIAN. ) SOLID_ANGLE_UNIT ( ) );
#3584 = ORIENTED_EDGE ( 'NONE', *, *, #12499, .T. ) ;
#3585 = CARTESIAN_POINT ( 'NONE',  ( 4.000000000000000000, -0.8732470631449981147, -3.223155494240760088 ) ) ;
#3586 = ORIENTED_EDGE ( 'NONE', *, *, #437, .F. ) ;
#3587 = EDGE_LOOP ( 'NONE', ( #3437, #15387, #13232, #5362, #6922, #8413, #13387, #9883, #9796, #1948, #5504, #9724, #4012, #3081, #7745, #357, #8664, #12813, #11686, #776, #7888, #484, #2349, #7079 ) ) ;
#3588 = ORIENTED_EDGE ( 'NONE', *, *, #13516, .T. ) ;
#3589 = CARTESIAN_POINT ( 'NONE',  ( 0.5093500532425063732, 4.799145180956616130, -3.374999998634407916 ) ) ;
#3590 = DIRECTION ( 'NONE',  ( 0.000000000000000000, 0.000000000000000000, -1.000000000000000000 ) ) ;
#3591 = AXIS2_PLACEMENT_3D ( 'NONE', #15304, #6421, #10055 ) ;
#3592 = CARTESIAN_POINT ( 'NONE',  ( -9.184850993605147944E-16, -29.25000000000000000, 5.000000000000000000 ) ) ;
#3593 = FACE_OUTER_BOUND ( 'NONE', #1006, .T. ) ;
#3594 = CYLINDRICAL_SURFACE ( 'NONE', #5991, 2.500000000000000888 ) ;
#3595 = CARTESIAN_POINT ( 'NONE',  ( 6.000000000000000000, -13.00000000000000178, -1.500000000000000000 ) ) ;
#3596 = CARTESIAN_POINT ( 'NONE',  ( 3.401574460001763001, -4.209348295687703967, -1.062499997268813612 ) ) ;
#3597 = DIRECTION ( 'NONE',  ( -0.000000000000000000, 1.000000000000000000, -0.000000000000000000 ) ) ;
#3598 =( NAMED_UNIT ( * ) PLANE_ANGLE_UNIT ( ) SI_UNIT ( $, .RADIAN. ) );
#3599 = CARTESIAN_POINT ( 'NONE',  ( 4.458734124999999437, -24.62500000136559564, -1.846868145590734978 ) ) ;
#3600 = CARTESIAN_POINT ( 'NONE',  ( -3.152801135295367096, -23.06250000136559564, -3.152801135295367541 ) ) ;
#3601 = CARTESIAN_POINT ( 'NONE',  ( -2.131511515620587272, -3.916244202832140253, -5.687499998634406140 ) ) ;
#3602 = CARTESIAN_POINT ( 'NONE',  ( -4.211140560182196957, 2.431303136016537803, -3.745885042887433514 ) ) ;
#3603 = ORIENTED_EDGE ( 'NONE', *, *, #11316, .F. ) ;
#3604 = ORIENTED_EDGE ( 'NONE', *, *, #2335, .T. ) ;
#3605 = ORIENTED_EDGE ( 'NONE', *, *, #9405, .T. ) ;
#3606 = CARTESIAN_POINT ( 'NONE',  ( -4.458734125000001214, -24.12500000136559919, 1.846868145590734089 ) ) ;
#3607 = LINE ( 'NONE', #7100, #1961 ) ;
#3608 = FACE_BOUND ( 'NONE', #15163, .T. ) ;
#3609 = APPLICATION_CONTEXT ( 'automotive_design' ) ;
#3610 = EDGE_CURVE ( 'NONE', #13050, #2328, #2566, .T. ) ;
#3611 = CARTESIAN_POINT ( 'NONE',  ( -15.99999999999979217, -9.000000000000001776, -1.500000000000001110 ) ) ;
#3612 = FACE_BOUND ( 'NONE', #11613, .T. ) ;
#3613 = EDGE_CURVE ( 'NONE', #12316, #14284, #839, .T. ) ;
#3614 = CARTESIAN_POINT ( 'NONE',  ( 2.071067811865476394, -23.18750000000000000, 5.000000000000000000 ) ) ;
#3615 = CARTESIAN_POINT ( 'NONE',  ( -2.390265326283148806, -4.391654775818394363, 0.6249999999999971134 ) ) ;
#3616 = DIRECTION ( 'NONE',  ( 0.000000000000000000, -0.5000000000000012212, -0.8660254037844380415 ) ) ;
#3617 = CARTESIAN_POINT ( 'NONE',  ( -9.184850993605147944E-16, -29.25000000000000000, 5.000000000000000000 ) ) ;
#3618 = CARTESIAN_POINT ( 'NONE',  ( -4.458734125000001214, -25.87500000136559919, 1.846868145590734089 ) ) ;
#3619 = B_SPLINE_CURVE_WITH_KNOTS ( 'NONE', 3,
 ( #12756, #3961, #8911, #13812, #5259, #7704, #6558, #1700, #7786, #4040, #11473, #421, #5347, #3083, #9229, #581 ),
 .UNSPECIFIED., .F., .F.,
 ( 4, 2, 2, 2, 2, 2, 2, 4 ),
 ( 8.673617379884034509E-19, 0.0003988053453839040001, 0.0007976106907678071328, 0.001196416036151710157, 0.001595221381535612314, 0.002392832072303412074, 0.002791637417687314882, 0.003190442763071217255 ),
 .UNSPECIFIED. ) ;
#3620 = CARTESIAN_POINT ( 'NONE',  ( 3.033343224707661712, -3.753672977998669946, -2.749999998634409248 ) ) ;
#3621 = ORIENTED_EDGE ( 'NONE', *, *, #2426, .F. ) ;
#3622 = CARTESIAN_POINT ( 'NONE',  ( 0.000000000000000000, 40.00000000000000000, 0.000000000000000000 ) ) ;
#3623 = ORIENTED_EDGE ( 'NONE', *, *, #6577, .F. ) ;
#3624 = ORIENTED_EDGE ( 'NONE', *, *, #3631, .F. ) ;
#3625 = CARTESIAN_POINT ( 'NONE',  ( -7.908228835406504231, 3.123118350879575456, -7.776694659841331791 ) ) ;
#3626 = CARTESIAN_POINT ( 'NONE',  ( -4.458734124999999437, -24.93750000136559564, -5.460374474430324690E-16 ) ) ;
#3627 = FACE_OUTER_BOUND ( 'NONE', #11745, .T. ) ;
#3628 = ORIENTED_EDGE ( 'NONE', *, *, #12871, .T. ) ;
#3629 = DIRECTION ( 'NONE',  ( 0.000000000000000000, 1.000000000000000000, 0.000000000000000000 ) ) ;
#3630 = DIRECTION ( 'NONE',  ( -0.000000000000000000, 1.471414886128461471E-15, 1.000000000000000000 ) ) ;
#3631 = EDGE_CURVE ( 'NONE', #15683, #15871, #5453, .T. ) ;
#3632 = CARTESIAN_POINT ( 'NONE',  ( 2.500000000000000000, 2.357898499370433054, -1.951563910473907981E-15 ) ) ;
#3633 = CARTESIAN_POINT ( 'NONE',  ( 17.99999999999957012, -8.784126309725975241E-13, 0.000000000000000000 ) ) ;
#3634 = EDGE_CURVE ( 'NONE', #3976, #15838, #34, .T. ) ;
#3635 = CARTESIAN_POINT ( 'NONE',  ( 3.152801135295366208, -24.81250000136559564, 3.152801135295367985 ) ) ;
#3636 = FACE_OUTER_BOUND ( 'NONE', #4460, .T. ) ;
#3637 = FACE_OUTER_BOUND ( 'NONE', #5751, .T. ) ;
#3638 = CARTESIAN_POINT ( 'NONE',  ( 5.000000000000000000, -28.12500000273118772, 0.000000000000000000 ) ) ;
#3639 = DIRECTION ( 'NONE',  ( 0.000000000000000000, 0.000000000000000000, -1.000000000000000000 ) ) ;
#3640 = CARTESIAN_POINT ( 'NONE',  ( -8.190561711645485556E-16, -30.68750000136559564, 4.458734124999999437 ) ) ;
#3641 = CARTESIAN_POINT ( 'NONE',  ( 9.184850993605153466E-15, 50.00000000000000000, 75.00000000000004263 ) ) ;
#3642 = ORIENTED_EDGE ( 'NONE', *, *, #9463, .T. ) ;
#3643 = VERTEX_POINT ( 'NONE', #3262 ) ;
#3644 = CARTESIAN_POINT ( 'NONE',  ( 35.00000000000000000, 37.00000000000000000, -8.572527594031472993E-15 ) ) ;
#3645 = VERTEX_POINT ( 'NONE', #3183 ) ;
#3646 = CARTESIAN_POINT ( 'NONE',  ( 0.000000000000000000, -13.00000000000000178, 0.000000000000000000 ) ) ;
#3647 = EDGE_CURVE ( 'NONE', #7141, #11376, #3344, .T. ) ;
#3648 = EDGE_CURVE ( 'NONE', #658, #7722, #9332, .T. ) ;
#3649 = DIRECTION ( 'NONE',  ( -0.000000000000000000, -1.000000000000000000, -0.000000000000000000 ) ) ;
#3650 = CARTESIAN_POINT ( 'NONE',  ( -4.799145180956616130, 0.5093500532425063732, -1.874999998634406584 ) ) ;
#3651 = AXIS2_PLACEMENT_3D ( 'NONE', #2260, #10529, #9467 ) ;
#3652 = SHAPE_DEFINITION_REPRESENTATION ( #10677, #10906 ) ;
#3653 =( BOUNDED_CURVE ( )  B_SPLINE_CURVE ( 2, ( #6121, #8631, #11049, #5606, #13525, #6450, #5222, #8792, #11362 ),
 .UNSPECIFIED., .F., .F. ) 
 B_SPLINE_CURVE_WITH_KNOTS ( ( 3, 2, 2, 2, 3 ),
 ( 0.3249999999999999556, 0.3374999999999999667, 0.3499999999999999778, 0.3624999999999999889, 0.3750000000000000000 ),
 .UNSPECIFIED. ) 
 CURVE ( )  GEOMETRIC_REPRESENTATION_ITEM ( )  RATIONAL_B_SPLINE_CURVE ( ( 1.000000000000000444, 0.9238795325112864054, 1.000000000000000000, 0.9238795325112867385, 1.000000000000000000, 0.9238795325112867385, 1.000000000000000000, 0.9238795325112867385, 1.000000000000000000 ) ) 
 REPRESENTATION_ITEM ( '' )  );
#3654 = CARTESIAN_POINT ( 'NONE',  ( -1.261996585732579224, 4.276409079477648589, -0.3124999986344085823 ) ) ;
#3655 = CARTESIAN_POINT ( 'NONE',  ( 2.071067811865476394, -24.18750000000000355, 5.000000000000000000 ) ) ;
#3656 = LINE ( 'NONE', #11098, #13351 ) ;
#3657 = SURFACE_STYLE_FILL_AREA ( #13668 ) ;
#3658 = ORIENTED_EDGE ( 'NONE', *, *, #7294, .T. ) ;
#3659 = CARTESIAN_POINT ( 'NONE',  ( -91.33974596215560382, -110.0591436588189396, 7.500000000000001776 ) ) ;
#3660 = EDGE_LOOP ( 'NONE', ( #15209, #2647, #3517, #8627, #809, #7575, #13814 ) ) ;
#3661 = ORIENTED_EDGE ( 'NONE', *, *, #12894, .F. ) ;
#3662 = CARTESIAN_POINT ( 'NONE',  ( -0.5093500532425060401, -4.799145180956616130, -3.874999998634408360 ) ) ;
#3663 = CARTESIAN_POINT ( 'NONE',  ( 6.123233995736766282E-16, -20.00000000000000000, -5.000000000000000000 ) ) ;
#3664 = EDGE_CURVE ( 'NONE', #9005, #13100, #13108, .T. ) ;
#3665 = ADVANCED_FACE ( 'NONE', ( #15396 ), #5528, .F. ) ;
#3666 = CARTESIAN_POINT ( 'NONE',  ( 4.276409079477644148, 1.261996585732577891, -8.312499998634407916 ) ) ;
#3667 = CARTESIAN_POINT ( 'NONE',  ( -7.500000000000005329, 4.330127018922194537, -9.999999999999998224 ) ) ;
#3668 = CARTESIAN_POINT ( 'NONE',  ( -9.184850993605147944E-16, -26.37500000273118417, 5.000000000000000000 ) ) ;
#3669 = CARTESIAN_POINT ( 'NONE',  ( 0.000000000000000000, -20.00000000000000000, 0.000000000000000000 ) ) ;
#3670 = CARTESIAN_POINT ( 'NONE',  ( 4.209348295687701302, 3.401574460001765665, -0.8124999972688135008 ) ) ;
#3671 = CARTESIAN_POINT ( 'NONE',  ( -21.01110699893060030, 0.000000000000000000, 36.39230484541324273 ) ) ;
#3672 = CARTESIAN_POINT ( 'NONE',  ( -4.458734124999999437, -25.18750000136559564, -5.460374474430324690E-16 ) ) ;
#3673 = CARTESIAN_POINT ( 'NONE',  ( 5.200000000000002842, 0.000000000000000000, 0.000000000000000000 ) ) ;
#3674 = CARTESIAN_POINT ( 'NONE',  ( -3.753672977998669946, -3.033343224707661712, -5.749999998634407916 ) ) ;
#3675 = AXIS2_PLACEMENT_3D ( 'NONE', #11479, #12607, #6561 ) ;
#3676 = DIRECTION ( 'NONE',  ( -1.000000000000000000, 0.000000000000000000, 0.000000000000000000 ) ) ;
#3677 = ORIENTED_EDGE ( 'NONE', *, *, #7275, .F. ) ;
#3678 = ORIENTED_EDGE ( 'NONE', *, *, #7728, .T. ) ;
#3679 = DIRECTION ( 'NONE',  ( 1.000000000000000000, 0.000000000000000000, 0.000000000000000000 ) ) ;
#3680 = ORIENTED_EDGE ( 'NONE', *, *, #12862, .T. ) ;
#3681 = CARTESIAN_POINT ( 'NONE',  ( 4.458734124999999437, -22.68750000136559564, 0.000000000000000000 ) ) ;
#3682 = CARTESIAN_POINT ( 'NONE',  ( 27.49999999999998224, -5.000000000000000000, 47.63139720814412925 ) ) ;
#3683 = CARTESIAN_POINT ( 'NONE',  ( 5.000000000000000000, -30.18750000273118417, 2.071067811865478614 ) ) ;
#3684 = EDGE_CURVE ( 'NONE', #10705, #12397, #9407, .T. ) ;
#3685 = AXIS2_PLACEMENT_3D ( 'NONE', #8899, #15040, #502 ) ;
#3686 = AXIS2_PLACEMENT_3D ( 'NONE', #6471, #1444, #10349 ) ;
#3687 = DIRECTION ( 'NONE',  ( 0.000000000000000000, -0.000000000000000000, 1.000000000000000000 ) ) ;
#3688 = DIRECTION ( 'NONE',  ( 0.000000000000000000, 0.000000000000000000, 1.000000000000000000 ) ) ;
#3689 = CARTESIAN_POINT ( 'NONE',  ( 1.415196051561583790, -4.795541693661363958, -2.250000000000001776 ) ) ;
#3690 = DIRECTION ( 'NONE',  ( -1.000000000000000000, -0.000000000000000000, -0.000000000000000000 ) ) ;
#3691 = CARTESIAN_POINT ( 'NONE',  ( -1.154700538379255903, 88.59290746114278647, 34.00000000000000711 ) ) ;
#3692 = CARTESIAN_POINT ( 'NONE',  ( 4.458734124999999437, -25.50000000136559919, 1.846868145590737864 ) ) ;
#3693 = CARTESIAN_POINT ( 'NONE',  ( -4.799145180956616130, 0.5093500532425063732, -4.124999998634405252 ) ) ;
#3694 = VERTEX_POINT ( 'NONE', #8048 ) ;
#3695 = CARTESIAN_POINT ( 'NONE',  ( 79.38739406438118351, 1.999999999999998224, 12.50099999999964417 ) ) ;
#3696 = ORIENTED_EDGE ( 'NONE', *, *, #11636, .T. ) ;
#3697 = MANIFOLD_SOLID_BREP ( 'Boss-Extrude3', #13843 ) ;
#3698 = VERTEX_POINT ( 'NONE', #7149 ) ;
#3699 = CARTESIAN_POINT ( 'NONE',  ( -7.500000000002755129, -3.882691789159864459, -7.781695678275425188 ) ) ;
#3700 = CARTESIAN_POINT ( 'NONE',  ( -1.846868145590737420, -26.75000000136559564, 4.458734124999999437 ) ) ;
#3701 = EDGE_CURVE ( 'NONE', #3157, #4598, #8127, .T. ) ;
#3702 = DIRECTION ( 'NONE',  ( 1.000000000000000000, 0.000000000000000000, -0.000000000000000000 ) ) ;
#3703 = ORIENTED_EDGE ( 'NONE', *, *, #14672, .F. ) ;
#3704 = DIRECTION ( 'NONE',  ( -1.000000000000000000, 0.000000000000000000, 0.000000000000000000 ) ) ;
#3705 = DIRECTION ( 'NONE',  ( -0.000000000000000000, -1.000000000000000000, -0.000000000000000000 ) ) ;
#3706 = FACE_BOUND ( 'NONE', #13137, .T. ) ;
#3707 = DIRECTION ( 'NONE',  ( -0.000000000000000000, -1.000000000000000000, -0.000000000000000000 ) ) ;
#3708 = CARTESIAN_POINT ( 'NONE',  ( 3.152801135295367541, -25.56250000136559564, -3.152801135295367541 ) ) ;
#3709 = FACE_OUTER_BOUND ( 'NONE', #12234, .T. ) ;
#3710 = CARTESIAN_POINT ( 'NONE',  ( -4.209348295687703079, -3.401574460001763445, -1.312499997268813834 ) ) ;
#3711 = CARTESIAN_POINT ( 'NONE',  ( 2.071067811865475505, -27.93750000273119127, -5.000000000000000888 ) ) ;
#3712 = CARTESIAN_POINT ( 'NONE',  ( 67.49999999999931788, 37.00000000000000000, 2.650000000000006573 ) ) ;
#3713 = COLOUR_RGB ( '', 0.72549020, 0.75294118, 0.79215686) ;
#3714 = CARTESIAN_POINT ( 'NONE',  ( 4.458734124999999437, -30.37500000136559564, -1.846868145590734978 ) ) ;
#3715 = PLANE ( 'NONE',  #15899 ) ;
#3716 = EDGE_LOOP ( 'NONE', ( #7241, #1780, #13245, #7331, #8705, #15659, #3805 ) ) ;
#3717 = AXIS2_PLACEMENT_3D ( 'NONE', #10186, #2978, #7932 ) ;
#3718 = FILL_AREA_STYLE ('',( #15857 ) ) ;
#3720 = ORIENTED_EDGE ( 'NONE', *, *, #13971, .T. ) ;
#3719 = EDGE_CURVE ( 'NONE', #7205, #13141, #10135, .T. ) ;
#3721 = PLANE ( 'NONE',  #2723 ) ;
#3722 = EDGE_CURVE ( 'NONE', #2036, #5406, #9562, .T. ) ;
#3723 = EDGE_LOOP ( 'NONE', ( #14344, #10607, #10726, #10650 ) ) ;
#3724 = CARTESIAN_POINT ( 'NONE',  ( 19.99999999999956657, -8.786575603324269439E-13, -13.00000000000000000 ) ) ;
#3725 = CIRCLE ( 'NONE', #7103, 2.649999999999985700 ) ;
#3726 = CARTESIAN_POINT ( 'NONE',  ( 4.999999999999845457, -1.272547481429021854, -3.961597479913466557 ) ) ;
#3727 = CARTESIAN_POINT ( 'NONE',  ( 4.799145180956616130, -0.5093500532425063732, -3.374999998634407472 ) ) ;
#3728 = CARTESIAN_POINT ( 'NONE',  ( -2.131511515620587272, -3.916244202832140253, -3.937499998634408360 ) ) ;
#3729 = CARTESIAN_POINT ( 'NONE',  ( 0.000000000000000000, -20.00000000000000000, 0.000000000000000000 ) ) ;
#3730 = DIRECTION ( 'NONE',  ( -0.4999999999999997224, 0.000000000000000000, -0.8660254037844388186 ) ) ;
#3731 = CIRCLE ( 'NONE', #8410, 2.041999999999999815 ) ;
#3732 = SURFACE_SIDE_STYLE ('',( #3657 ) ) ;
#3733 = ADVANCED_FACE ( 'NONE', ( #13488 ), #11968, .F. ) ;
#3734 = ORIENTED_EDGE ( 'NONE', *, *, #14085, .T. ) ;
#3735 = CARTESIAN_POINT ( 'NONE',  ( 4.000000000000000000, 0.8378280264232961239, -3.220590601395640018 ) ) ;
#3736 = DIRECTION ( 'NONE',  ( -0.005931855436079598413, 0.9999824063907751803, 0.000000000000000000 ) ) ;
#3737 = ADVANCED_FACE ( 'NONE', ( #10931 ), #6004, .F. ) ;
#3738 = AXIS2_PLACEMENT_3D ( 'NONE', #10847, #8286, #9481 ) ;
#3739 = ORIENTED_EDGE ( 'NONE', *, *, #8722, .F. ) ;
#3740 = CONTEXT_DEPENDENT_SHAPE_REPRESENTATION ( #6927, #7535 ) ;
#3741 = CARTESIAN_POINT ( 'NONE',  ( 3.916244202832140253, -2.131511515620588160, -4.687499998634405252 ) ) ;
#3742 = LINE ( 'NONE', #2519, #1941 ) ;
#3743 = AXIS2_PLACEMENT_3D ( 'NONE', #2244, #6964, #10667 ) ;
#3744 = CARTESIAN_POINT ( 'NONE',  ( -1.261996585732579224, 4.276409079477648589, -8.062499998634407916 ) ) ;
#3745 = DIRECTION ( 'NONE',  ( -0.000000000000000000, 1.000000000000000000, -0.000000000000000000 ) ) ;
#3746 = CYLINDRICAL_SURFACE ( 'NONE', #4364, 10.00000000000000178 ) ;
#3747 = CARTESIAN_POINT ( 'NONE',  ( -4.795541693661363958, -1.415196051561583790, -3.374999997268816276 ) ) ;
#3748 = DIRECTION ( 'NONE',  ( -0.000000000000000000, -1.000000000000000000, -0.000000000000000000 ) ) ;
#3749 = CARTESIAN_POINT ( 'NONE',  ( -5.725490332106780933, -3.000000000000000000, -9.916840153467775920 ) ) ;
#3750 = CARTESIAN_POINT ( 'NONE',  ( -4.458734125000000326, -25.12500000136559564, 1.846868145590734089 ) ) ;
#3751 = ORIENTED_EDGE ( 'NONE', *, *, #3382, .T. ) ;
#3752 = CARTESIAN_POINT ( 'NONE',  ( -86.33974596215563224, -97.11324865405184426, -7.500000000000000000 ) ) ;
#3753 = CARTESIAN_POINT ( 'NONE',  ( -3.916244202832140253, 2.131511515620587272, -4.937499998634406140 ) ) ;
#3754 = DIRECTION ( 'NONE',  ( 1.000000000000000000, -0.000000000000000000, -1.239088197126290570E-16 ) ) ;
#3755 = ADVANCED_FACE ( 'NONE', ( #3577 ), #2198, .T. ) ;
#3756 = ORIENTED_EDGE ( 'NONE', *, *, #2865, .F. ) ;
#3757 = EDGE_LOOP ( 'NONE', ( #11136, #9700, #964, #2413 ) ) ;
#3758 = ADVANCED_FACE ( 'NONE', ( #15869 ), #4791, .T. ) ;
#3759 = ADVANCED_FACE ( 'NONE', ( #9632 ), #13182, .F. ) ;
#3761 = CONICAL_SURFACE ( 'NONE', #5586, 7.500000000000001776, 0.8594454914424796144 ) ;
#3760 = DIRECTION ( 'NONE',  ( 1.000000000000000000, 0.000000000000000000, 0.000000000000000000 ) ) ;
#3762 = ORIENTED_EDGE ( 'NONE', *, *, #14528, .F. ) ;
#3763 = CARTESIAN_POINT ( 'NONE',  ( 3.152801135295366208, -22.81250000136559564, 3.152801135295367985 ) ) ;
#3764 = LINE ( 'NONE', #7500, #9971 ) ;
#3765 = VECTOR ( 'NONE', #329, 1000.000000000000000 ) ;
#3766 = DIRECTION ( 'NONE',  ( 0.000000000000000000, -0.000000000000000000, 1.000000000000000000 ) ) ;
#3767 = CARTESIAN_POINT ( 'NONE',  ( -9.184850993605147944E-16, -26.25000000000000355, 5.000000000000000000 ) ) ;
#3768 = DIRECTION ( 'NONE',  ( 0.000000000000000000, 0.000000000000000000, 1.000000000000000000 ) ) ;
#3769 = PLANE ( 'NONE',  #9018 ) ;
#3770 = VECTOR ( 'NONE', #10560, 1000.000000000000000 ) ;
#3771 = CARTESIAN_POINT ( 'NONE',  ( -0.5711823568785978633, -5.381735091635035495, -0.3124999999999993339 ) ) ;
#3772 = CARTESIAN_POINT ( 'NONE',  ( 5.000000000000004441, 6.350331166892669572E-15, -1.920263044861758583 ) ) ;
#3773 = DIRECTION ( 'NONE',  ( 0.000000000000000000, 0.000000000000000000, 1.000000000000000000 ) ) ;
#3774 = CARTESIAN_POINT ( 'NONE',  ( 4.458734125000000326, -28.37500000136559564, -1.846868145590734978 ) ) ;
#3775 = AXIS2_PLACEMENT_3D ( 'NONE', #11513, #4244, #1894 ) ;
#3776 = CARTESIAN_POINT ( 'NONE',  ( -1.261996585732579224, 4.276409079477648589, -3.312499998634407916 ) ) ;
#3777 = ORIENTED_EDGE ( 'NONE', *, *, #1820, .F. ) ;
#3778 = CARTESIAN_POINT ( 'NONE',  ( -7.500000000000007105, -1.486698507076798181, -0.09861472150524400182 ) ) ;
#3779 = VERTEX_POINT ( 'NONE', #12205 ) ;
#3780 = MANIFOLD_SOLID_BREP ( 'Cavity1', #6630 ) ;
#3781 = VERTEX_POINT ( 'NONE', #7380 ) ;
#3782 = CARTESIAN_POINT ( 'NONE',  ( -3.999999999998910649, -1.658469974638591804, -3.531532913075256186 ) ) ;
#3783 = EDGE_CURVE ( 'NONE', #6940, #1967, #11009, .T. ) ;
#3784 = CARTESIAN_POINT ( 'NONE',  ( -1.846868145590737420, -25.75000000136559564, 4.458734124999999437 ) ) ;
#3785 = DIRECTION ( 'NONE',  ( 0.000000000000000000, 0.000000000000000000, -1.000000000000000000 ) ) ;
#3786 = VECTOR ( 'NONE', #7903, 1000.000000000000000 ) ;
#3787 = VERTEX_POINT ( 'NONE', #14980 ) ;
#3788 = DIRECTION ( 'NONE',  ( 0.000000000000000000, 0.000000000000000000, 1.000000000000000000 ) ) ;
#3789 = AXIS2_PLACEMENT_3D ( 'NONE', #3392, #4527, #3322 ) ;
#3790 = CARTESIAN_POINT ( 'NONE',  ( 3.288228914120474133, -7.217643567644815406, -7.591235721156640359 ) ) ;
#3791 = PLANE ( 'NONE',  #15961 ) ;
#3792 = CARTESIAN_POINT ( 'NONE',  ( 0.000000000000000000, -13.00000000000000178, 0.000000000000000000 ) ) ;
#3793 = CARTESIAN_POINT ( 'NONE',  ( -5.000000000000000000, -28.50000000000000000, -6.123233995736766282E-16 ) ) ;
#3794 = FACE_BOUND ( 'NONE', #6920, .T. ) ;
#3795 = ADVANCED_FACE ( 'NONE', ( #12612 ), #6330, .F. ) ;
#3796 = CIRCLE ( 'NONE', #14905, 2.499999999999999556 ) ;
#3797 = DIRECTION ( 'NONE',  ( 0.000000000000000000, 0.8660254037844380415, -0.5000000000000011102 ) ) ;
#3798 = CARTESIAN_POINT ( 'NONE',  ( -2.071067811865475061, -26.81250000273118417, -5.000000000000000888 ) ) ;
#3799 = CARTESIAN_POINT ( 'NONE',  ( 2.500000000000000000, -1.178949249685213863, 2.042000000000002924 ) ) ;
#3800 = CARTESIAN_POINT ( 'NONE',  ( 3.535533905932738197, -24.00000000273118772, -3.535533905932738197 ) ) ;
#3801 =( NAMED_UNIT ( * ) PLANE_ANGLE_UNIT ( ) SI_UNIT ( $, .RADIAN. ) );
#3802 = ORIENTED_EDGE ( 'NONE', *, *, #15234, .F. ) ;
#3803 = VERTEX_POINT ( 'NONE', #107 ) ;
#3804 = CARTESIAN_POINT ( 'NONE',  ( -90.00000000000000000, -35.00000000000000711, 7.500000000000001776 ) ) ;
#3805 = ORIENTED_EDGE ( 'NONE', *, *, #566, .T. ) ;
#3806 = CARTESIAN_POINT ( 'NONE',  ( -35.00000000000000000, 37.00000000000000000, -2.649999999999992806 ) ) ;
#3807 = AXIS2_PLACEMENT_3D ( 'NONE', #10614, #6741, #11641 ) ;
#3808 = DIRECTION ( 'NONE',  ( 0.000000000000000000, -0.4999999999999993894, 0.8660254037844389297 ) ) ;
#3809 = CIRCLE ( 'NONE', #724, 2.000000000000000888 ) ;
#3810 = ADVANCED_FACE ( 'NONE', ( #7468, #13914, #7548 ), #3892, .T. ) ;
#3811 = CARTESIAN_POINT ( 'NONE',  ( 4.276409079477644148, 1.261996585732577891, -4.312499998634405252 ) ) ;
#3812 = EDGE_CURVE ( 'NONE', #7875, #12489, #3398, .T. ) ;
#3813 = CARTESIAN_POINT ( 'NONE',  ( 35.00000000000000000, 55.00000000000000711, 2.444036937190193601E-13 ) ) ;
#3814 = CARTESIAN_POINT ( 'NONE',  ( -4.276409079477644148, -1.261996585732578335, -6.062499998634407028 ) ) ;
#3815 = CARTESIAN_POINT ( 'NONE',  ( 0.000000000000000000, -20.00000000000000000, 0.000000000000000000 ) ) ;
#3816 = CIRCLE ( 'NONE', #10021, 6.000000000000000888 ) ;
#3817 = CYLINDRICAL_SURFACE ( 'NONE', #6946, 9.999999999999992895 ) ;
#3818 = ORIENTED_EDGE ( 'NONE', *, *, #12542, .F. ) ;
#3819 = CARTESIAN_POINT ( 'NONE',  ( 3.137352903976079244, -3.012258285427876547, -48.92283135131768290 ) ) ;
#3820 = AXIS2_PLACEMENT_3D ( 'NONE', #10472, #10010, #9105 ) ;
#3821 = FILL_AREA_STYLE_COLOUR ( '', #6625 ) ;
#3822 = ORIENTED_EDGE ( 'NONE', *, *, #12125, .F. ) ;
#3823 = DIRECTION ( 'NONE',  ( 0.000000000000000000, 0.000000000000000000, 1.000000000000000000 ) ) ;
#3824 = LINE ( 'NONE', #8927, #13058 ) ;
#3825 = VECTOR ( 'NONE', #7444, 1000.000000000000114 ) ;
#3826 = ORIENTED_EDGE ( 'NONE', *, *, #5340, .F. ) ;
#3827 = CARTESIAN_POINT ( 'NONE',  ( -3.916244202832140253, 2.131511515620587272, -8.187499998634407916 ) ) ;
#3828 = CARTESIAN_POINT ( 'NONE',  ( -5.000000000000004441, -1.011557177027151181E-15, -4.420263044861760804 ) ) ;
#3829 = CIRCLE ( 'NONE', #5397, 4.250000000000000000 ) ;
#3830 = LINE ( 'NONE', #14742, #9275 ) ;
#3831 = CARTESIAN_POINT ( 'NONE',  ( -5.384454397937118664, 6.702023979852544604E-16, -5.000000000000000000 ) ) ;
#3832 = EDGE_CURVE ( 'NONE', #14231, #15006, #11260, .T. ) ;
#3833 = PRODUCT_DEFINITION_CONTEXT ( 'detailed design', #1957, 'design' ) ;
#3834 = DIRECTION ( 'NONE',  ( 0.000000000000000000, 0.000000000000000000, 1.000000000000000000 ) ) ;
#3835 = VECTOR ( 'NONE', #8593, 1000.000000000000000 ) ;
#3836 = CARTESIAN_POINT ( 'NONE',  ( 5.381735091635035495, -0.5711823568785978633, -3.937499997268818497 ) ) ;
#3837 = CARTESIAN_POINT ( 'NONE',  ( 5.000000000000000888, 0.000000000000000000, 0.000000000000000000 ) ) ;
#3838 = CARTESIAN_POINT ( 'NONE',  ( -2.533142440694107655, 3.791257988497170661, -0.3164060562859182801 ) ) ;
#3839 = CARTESIAN_POINT ( 'NONE',  ( -3.152801135295367985, -26.06250000136559919, 3.152801135295367096 ) ) ;
#3840 = ORIENTED_EDGE ( 'NONE', *, *, #8774, .F. ) ;
#3841 = DIRECTION ( 'NONE',  ( -0.000000000000000000, -0.000000000000000000, -1.000000000000000000 ) ) ;
#3842 = CARTESIAN_POINT ( 'NONE',  ( 4.276409079477644148, 1.261996585732577891, -2.312499998634407028 ) ) ;
#3843 = CARTESIAN_POINT ( 'NONE',  ( -4.101948962585906244, 2.368261337751074169, -3.681124513963621503 ) ) ;
#3844 = ORIENTED_EDGE ( 'NONE', *, *, #5702, .F. ) ;
#3845 = AXIS2_PLACEMENT_3D ( 'NONE', #12116, #10995, #15934 ) ;
#3846 = ORIENTED_EDGE ( 'NONE', *, *, #7499, .T. ) ;
#3847 = AXIS2_PLACEMENT_3D ( 'NONE', #5001, #8735, #1442 ) ;
#3848 = ORIENTED_EDGE ( 'NONE', *, *, #1278, .F. ) ;
#3849 = CARTESIAN_POINT ( 'NONE',  ( 1.846868145590735200, -23.50000000136559564, -4.458734125000000326 ) ) ;
#3850 = DIRECTION ( 'NONE',  ( 0.000000000000000000, 0.000000000000000000, 1.000000000000000000 ) ) ;
#3851 =( BOUNDED_CURVE ( )  B_SPLINE_CURVE ( 2, ( #9369, #4273, #5490, #14138, #13217, #8165, #14293, #9445, #13148, #10507, #11693 ),
 .UNSPECIFIED., .F., .F. ) 
 B_SPLINE_CURVE_WITH_KNOTS ( ( 3, 2, 2, 2, 2, 3 ),
 ( 0.6545872658012773515, 0.6624999999999999778, 0.6750000000000000444, 0.6875000000000000000, 0.6999999999999999556, 0.7045872658012772849 ),
 .UNSPECIFIED. ) 
 CURVE ( )  GEOMETRIC_REPRESENTATION_ITEM ( )  RATIONAL_B_SPLINE_CURVE ( ( 0.9646335149384803742, 0.9518143178943441196, 1.000000000000000000, 0.9238795325112867385, 1.000000000000000000, 0.9238795325112867385, 1.000000000000000000, 0.9238795325112867385, 1.000000000000000000, 0.9720652146169428409, 0.9646335149384808183 ) ) 
 REPRESENTATION_ITEM ( '' )  );
#3852 = CARTESIAN_POINT ( 'NONE',  ( 0.000000000000000000, -13.00000000000000178, 0.000000000000000000 ) ) ;
#3853 = EDGE_CURVE ( 'NONE', #5290, #11740, #4337, .T. ) ;
#3854 = CARTESIAN_POINT ( 'NONE',  ( 2.071067811865462183, -26.18750000000000711, 5.000000000000013323 ) ) ;
#3855 = CARTESIAN_POINT ( 'NONE',  ( -2.411464220262878655, -7.267994521134962582, -7.491772860716182869 ) ) ;
#3856 = ADVANCED_FACE ( 'NONE', ( #12448 ), #11484, .F. ) ;
#3857 = CARTESIAN_POINT ( 'NONE',  ( -116.3391301858327438, -120.2076149402627152, 13.35786437626905965 ) ) ;
#3858 = CARTESIAN_POINT ( 'NONE',  ( -4.795541693661363958, -1.415196051561583790, -4.500000000000000888 ) ) ;
#3859 = CARTESIAN_POINT ( 'NONE',  ( 0.000000000000000000, -20.00000000000000000, 0.000000000000000000 ) ) ;
#3860 = DIRECTION ( 'NONE',  ( 1.000000000000000000, 0.000000000000000000, 0.000000000000000000 ) ) ;
#3861 = CARTESIAN_POINT ( 'NONE',  ( -4.458734124999999437, -24.93750000136559564, -5.460374474430324690E-16 ) ) ;
#3862 = CARTESIAN_POINT ( 'NONE',  ( -4.799145180956616130, 0.5093500532425063732, -3.124999998634407916 ) ) ;
#3863 = ORIENTED_EDGE ( 'NONE', *, *, #14819, .F. ) ;
#3864 = CARTESIAN_POINT ( 'NONE',  ( -7.922281120364393914, -4.573931137438277617, -8.047472243342932430 ) ) ;
#3865 = ORIENTED_EDGE ( 'NONE', *, *, #7478, .F. ) ;
#3866 = ORIENTED_EDGE ( 'NONE', *, *, #5204, .T. ) ;
#3867 = DIRECTION ( 'NONE',  ( -0.000000000000000000, 1.000000000000000000, -0.000000000000000000 ) ) ;
#3868 = CARTESIAN_POINT ( 'NONE',  ( -8.190561711645485556E-16, -24.68750000136559564, 4.458734124999999437 ) ) ;
#3869 = LINE ( 'NONE', #7597, #3765 ) ;
#3870 = ORIENTED_EDGE ( 'NONE', *, *, #9426, .F. ) ;
#3871 = VECTOR ( 'NONE', #10384, 1000.000000000000114 ) ;
#3872 = CYLINDRICAL_SURFACE ( 'NONE', #14600, 2.000000000000000888 ) ;
#3873 = CYLINDRICAL_SURFACE ( 'NONE', #3847, 5.000000000000000000 ) ;
#3874 = CARTESIAN_POINT ( 'NONE',  ( 4.799145180956616130, -0.5093500532425063732, -3.374999998634407916 ) ) ;
#3875 = CARTESIAN_POINT ( 'NONE',  ( 2.337141007481793764, 3.806500215644827545, -0.3789984458506294174 ) ) ;
#3876 = ADVANCED_FACE ( 'NONE', ( #5026 ), #9956, .F. ) ;
#3877 = CARTESIAN_POINT ( 'NONE',  ( 3.061616997868383141E-16, -29.75000000000000000, -5.000000000000000000 ) ) ;
#3878 = CARTESIAN_POINT ( 'NONE',  ( -0.1756481739660520902, 4.720212674038980261, -3.469390959564065291 ) ) ;
#3879 = CARTESIAN_POINT ( 'NONE',  ( 16.49999999999956657, -8.782289339527253835E-13, -6.000000000000000000 ) ) ;
#3880 = CARTESIAN_POINT ( 'NONE',  ( -3.535533905932738641, -26.50000000273118772, 3.535533905932737309 ) ) ;
#3881 = CARTESIAN_POINT ( 'NONE',  ( 4.999999999999848121, -1.272547481429015859, -5.961597479913463893 ) ) ;
#3882 = CARTESIAN_POINT ( 'NONE',  ( -4.458734124999999437, -29.93750000136559564, -5.460374474430324690E-16 ) ) ;
#3883 = ORIENTED_EDGE ( 'NONE', *, *, #7227, .T. ) ;
#3884 = ORIENTED_EDGE ( 'NONE', *, *, #4510, .F. ) ;
#3885 = ORIENTED_EDGE ( 'NONE', *, *, #11570, .T. ) ;
#3886 = FACE_OUTER_BOUND ( 'NONE', #14080, .T. ) ;
#3887 = ORIENTED_EDGE ( 'NONE', *, *, #8774, .T. ) ;
#3888 = DIRECTION ( 'NONE',  ( 0.000000000000000000, 0.000000000000000000, 1.000000000000000000 ) ) ;
#3889 = FACE_OUTER_BOUND ( 'NONE', #3587, .T. ) ;
#3890 = APPLICATION_PROTOCOL_DEFINITION ( 'draft international standard', 'automotive_design', 1998, #7320 ) ;
#3891 = CARTESIAN_POINT ( 'NONE',  ( -0.5093500532425060401, -4.799145180956616130, -6.874999998634407916 ) ) ;
#3892 = PLANE ( 'NONE',  #8955 ) ;
#3893 = DIRECTION ( 'NONE',  ( -0.000000000000000000, -1.000000000000000000, -0.000000000000000000 ) ) ;
#3894 = EDGE_LOOP ( 'NONE', ( #8906, #760 ) ) ;
#3895 = FACE_OUTER_BOUND ( 'NONE', #6640, .T. ) ;
#3896 = VERTEX_POINT ( 'NONE', #12372 ) ;
#3897 = CARTESIAN_POINT ( 'NONE',  ( -41.99999999999978684, -9.000000000000001776, 3.499999999999998668 ) ) ;
#3898 = DIRECTION ( 'NONE',  ( 0.000000000000000000, 1.000000000000000000, 0.000000000000000000 ) ) ;
#3899 = ORIENTED_EDGE ( 'NONE', *, *, #1875, .T. ) ;
#3900 = ITEM_DEFINED_TRANSFORMATION ( 'NONE', 'NONE', #15612,  #3223 ) ;
#3901 = CARTESIAN_POINT ( 'NONE',  ( 3.753672977998667726, 3.033343224707664820, -7.499999998634409692 ) ) ;
#3902 = EDGE_CURVE ( 'NONE', #6035, #6779, #12054, .T. ) ;
#3903 = PRESENTATION_STYLE_ASSIGNMENT (( #1488 ) ) ;
#3904 = PRODUCT_DEFINITION_SHAPE ( 'NONE', 'NONE',  #15998 ) ;
#3905 = CARTESIAN_POINT ( 'NONE',  ( -5.000000000000000888, -28.68750000273119127, -2.071067811865475949 ) ) ;
#3906 = DIRECTION ( 'NONE',  ( 0.000000000000000000, 0.000000000000000000, 1.000000000000000000 ) ) ;
#3907 = FACE_OUTER_BOUND ( 'NONE', #2286, .T. ) ;
#3908 = CARTESIAN_POINT ( 'NONE',  ( 4.209348295687701302, 3.401574460001765665, -3.812499997268815832 ) ) ;
#3909 = CARTESIAN_POINT ( 'NONE',  ( -3.401574460001765221, 4.209348295687701302, -8.562499997268812280 ) ) ;
#3910 =( REPRESENTATION_RELATIONSHIP ('NONE','NONE', #4176, #3173 ) REPRESENTATION_RELATIONSHIP_WITH_TRANSFORMATION ( #5355 )SHAPE_REPRESENTATION_RELATIONSHIP( ) );
#3911 = CARTESIAN_POINT ( 'NONE',  ( -3.293006400480308127, 3.192677401847128671, -0.2974341898043406651 ) ) ;
#3912 = CARTESIAN_POINT ( 'NONE',  ( 4.458734124999999437, -22.62500000136559564, -1.846868145590734978 ) ) ;
#3913 = ORIENTED_EDGE ( 'NONE', *, *, #4216, .F. ) ;
#3914 = DIRECTION ( 'NONE',  ( -0.000000000000000000, -1.000000000000000000, -0.000000000000000000 ) ) ;
#3915 = FACE_BOUND ( 'NONE', #5233, .T. ) ;
#3916 = CARTESIAN_POINT ( 'NONE',  ( -4.000000000000000000, 2.309401076758498483, -3.433295621305379353 ) ) ;
#3917 = ORIENTED_EDGE ( 'NONE', *, *, #7796, .F. ) ;
#3918 = VERTEX_POINT ( 'NONE', #10209 ) ;
#3919 = CIRCLE ( 'NONE', #8071, 5.000000000000000000 ) ;
#3920 = VERTEX_POINT ( 'NONE', #14896 ) ;
#3921 = CYLINDRICAL_SURFACE ( 'NONE', #8223, 5.000000000000000000 ) ;
#3922 = EDGE_CURVE ( 'NONE', #14864, #5642, #7921, .T. ) ;
#3923 = DIRECTION ( 'NONE',  ( 0.000000000000000000, 0.000000000000000000, 1.000000000000000000 ) ) ;
#3924 = ADVANCED_FACE ( 'NONE', ( #5112 ), #8837, .T. ) ;
#3925 = CARTESIAN_POINT ( 'NONE',  ( 0.5789871446316211534, 4.420982230657665824, -0.3789984458506777676 ) ) ;
#3926 = CARTESIAN_POINT ( 'NONE',  ( -5.274401269815138349, -6.074457022762090652, -7.633824513837112136 ) ) ;
#3927 = FACE_OUTER_BOUND ( 'NONE', #8623, .T. ) ;
#3928 = LINE ( 'NONE', #8873, #6690 ) ;
#3929 = CARTESIAN_POINT ( 'NONE',  ( 5.381735091635035495, -0.5711823568785978633, -5.062500000000000888 ) ) ;
#3930 = LINE ( 'NONE', #12806, #4979 ) ;
#3931 = VECTOR ( 'NONE', #7336, 1000.000000000000000 ) ;
#3932 = FACE_OUTER_BOUND ( 'NONE', #9636, .T. ) ;
#3933 = CARTESIAN_POINT ( 'NONE',  ( -3.152801135295367985, -23.81250000136559564, 3.152801135295367096 ) ) ;
#3934 = CARTESIAN_POINT ( 'NONE',  ( -0.5093500532425060401, -4.799145180956616130, -6.874999998634407916 ) ) ;
#3935 = ORIENTED_EDGE ( 'NONE', *, *, #11944, .T. ) ;
#3936 = CARTESIAN_POINT ( 'NONE',  ( -36.99999999999999289, -11.00000000000000178, -1.999999999999170885 ) ) ;
#3937 = ORIENTED_EDGE ( 'NONE', *, *, #7399, .F. ) ;
#3938 = ORIENTED_EDGE ( 'NONE', *, *, #100, .T. ) ;
#3939 = CARTESIAN_POINT ( 'NONE',  ( 3.152801135295367541, -29.56250000136559208, -3.152801135295367541 ) ) ;
#3940 = EDGE_CURVE ( 'NONE', #15165, #4719, #8920, .T. ) ;
#3941 = DIRECTION ( 'NONE',  ( 0.000000000000000000, 0.000000000000000000, 1.000000000000000000 ) ) ;
#3942 = EDGE_CURVE ( 'NONE', #138, #1457, #7143, .T. ) ;
#3943 = ORIENTED_EDGE ( 'NONE', *, *, #6047, .T. ) ;
#3944 = CIRCLE ( 'NONE', #850, 2.649999999999985700 ) ;
#3945 = CARTESIAN_POINT ( 'NONE',  ( 1.243802165048773611, -3.900692638707475624, -3.223146290109810241 ) ) ;
#3946 = AXIS2_PLACEMENT_3D ( 'NONE', #9061, #569, #12588 ) ;
#3947 = CARTESIAN_POINT ( 'NONE',  ( 10.12668159690567649, 0.000000000000000000, -9.226681596905677907 ) ) ;
#3948 = CARTESIAN_POINT ( 'NONE',  ( -4.799145180956616130, 0.5093500532425063732, -1.874999998634406584 ) ) ;
#3949 = DIRECTION ( 'NONE',  ( 0.000000000000000000, 0.000000000000000000, -1.000000000000000000 ) ) ;
#3950 = CARTESIAN_POINT ( 'NONE',  ( 3.535533905932738197, -29.87500000000000000, -3.535533905932738197 ) ) ;
#3951 = AXIS2_PLACEMENT_3D ( 'NONE', #319, #11443, #5229 ) ;
#3952 = CARTESIAN_POINT ( 'NONE',  ( -43.93697442715794210, -3.012271619929379085, -21.74475519031983950 ) ) ;
#3953 = LINE ( 'NONE', #10353, #7218 ) ;
#3954 = CARTESIAN_POINT ( 'NONE',  ( -2.071067811865478170, -29.43750000273118772, 5.000000000000000000 ) ) ;
#3955 = CARTESIAN_POINT ( 'NONE',  ( -5.000000000000095035, -0.7223674278660573433, -3.521799365517154001 ) ) ;
#3956 = ORIENTED_EDGE ( 'NONE', *, *, #10924, .F. ) ;
#3957 = ORIENTED_EDGE ( 'NONE', *, *, #2865, .T. ) ;
#3958 = B_SPLINE_CURVE_WITH_KNOTS ( 'NONE', 3,
 ( #7600, #12497, #1438, #6386, #7684, #11304 ),
 .UNSPECIFIED., .F., .F.,
 ( 4, 2, 4 ),
 ( 0.003358874760055550156, 0.004541967308452096383, 0.005725059856848641743 ),
 .UNSPECIFIED. ) ;
#3960 = ADVANCED_FACE ( 'NONE', ( #10124 ), #2761, .T. ) ;
#3959 = VERTEX_POINT ( 'NONE', #281 ) ;
#3961 = CARTESIAN_POINT ( 'NONE',  ( -44.43375672974056556, -4.865128266864608975, 19.99999999999999645 ) ) ;
#3962 = EDGE_CURVE ( 'NONE', #10453, #8590, #14879, .T. ) ;
#3963 = VERTEX_POINT ( 'NONE', #1865 ) ;
#3964 = CARTESIAN_POINT ( 'NONE',  ( 0.000000000000000000, 50.00000000000000000, 0.000000000000000000 ) ) ;
#3965 = CARTESIAN_POINT ( 'NONE',  ( 7.894787914004607998, 1.231001383561881556E-13, -7.591390474663423760 ) ) ;
#3966 = CARTESIAN_POINT ( 'NONE',  ( -1.846868145590737420, -30.00000000136559564, 4.458734124999999437 ) ) ;
#3967 = STYLED_ITEM ( 'NONE', ( #6161 ), #15834 ) ;
#3968 = CARTESIAN_POINT ( 'NONE',  ( 0.5093500532425063732, 4.799145180956616130, -7.374999998634408804 ) ) ;
#3969 = CARTESIAN_POINT ( 'NONE',  ( 0.000000000000000000, 0.000000000000000000, 0.000000000000000000 ) ) ;
#3970 = ORIENTED_EDGE ( 'NONE', *, *, #14575, .F. ) ;
#3971 = DIRECTION ( 'NONE',  ( 0.000000000000000000, 0.000000000000000000, 1.000000000000000000 ) ) ;
#3972 = VERTEX_POINT ( 'NONE', #13299 ) ;
#3973 = CARTESIAN_POINT ( 'NONE',  ( -115.0000000000000142, -10.00000000000000888, 7.500000000000001776 ) ) ;
#3974 = CARTESIAN_POINT ( 'NONE',  ( 2.143131898507869826E-15, 50.00000000000000000, -64.85000000000002274 ) ) ;
#3975 = EDGE_CURVE ( 'NONE', #12212, #9210, #15144, .T. ) ;
#3976 = VERTEX_POINT ( 'NONE', #15380 ) ;
#3977 = CARTESIAN_POINT ( 'NONE',  ( -1.261996585732579224, 4.276409079477648589, -7.312499998634407916 ) ) ;
#3978 = AXIS2_PLACEMENT_3D ( 'NONE', #2023, #5742, #9315 ) ;
#3979 =( NAMED_UNIT ( * ) SI_UNIT ( $, .STERADIAN. ) SOLID_ANGLE_UNIT ( ) );
#3980 = LINE ( 'NONE', #3408, #251 ) ;
#3981 = CARTESIAN_POINT ( 'NONE',  ( 67.49999999999931788, 50.00000000000000000, 2.650000000000013678 ) ) ;
#3982 = CARTESIAN_POINT ( 'NONE',  ( 4.896370289192182312, -5.000000000000000000, -48.48076211352908871 ) ) ;
#3983 = VECTOR ( 'NONE', #1727, 1000.000000000000000 ) ;
#3984 = CARTESIAN_POINT ( 'NONE',  ( -2.390265326283148806, -4.391654775818394363, -4.249999997268816720 ) ) ;
#3985 = CARTESIAN_POINT ( 'NONE',  ( 3.333333333333335702, -2.694301256218268215, -3.300726591567084256 ) ) ;
#3986 = EDGE_CURVE ( 'NONE', #8492, #8391, #4459, .T. ) ;
#3987 = LINE ( 'NONE', #7486, #8753 ) ;
#3988 = LINE ( 'NONE', #10070, #13013 ) ;
#3989 = EDGE_LOOP ( 'NONE', ( #2661, #5480, #10236, #6535, #8095, #97 ) ) ;
#3990 = CARTESIAN_POINT ( 'NONE',  ( -2.886751345948103342, -37.00000000000000711, -35.00000000000000000 ) ) ;
#3991 = CARTESIAN_POINT ( 'NONE',  ( -4.211140560182196957, 2.431303136016537803, -3.745885042887433514 ) ) ;
#3992 = DIRECTION ( 'NONE',  ( -0.000000000000000000, -0.000000000000000000, 1.000000000000000000 ) ) ;
#3993 = VERTEX_POINT ( 'NONE', #14319 ) ;
#3994 = ORIENTED_EDGE ( 'NONE', *, *, #9740, .F. ) ;
#3995 = EDGE_LOOP ( 'NONE', ( #1798, #13792, #7346, #5691 ) ) ;
#3996 = CYLINDRICAL_SURFACE ( 'NONE', #3031, 4.999999999999997335 ) ;
#3997 = FACE_OUTER_BOUND ( 'NONE', #13080, .T. ) ;
#3998 = STYLED_ITEM ( 'NONE', ( #4391 ), #6973 ) ;
#3999 = CARTESIAN_POINT ( 'NONE',  ( 47.32050807568875683, -37.00000000000000711, 41.96152422706633445 ) ) ;
#4000 = VECTOR ( 'NONE', #14821, 1000.000000000000000 ) ;
#4001 = APPLICATION_CONTEXT ( 'automotive_design' ) ;
#4002 = CARTESIAN_POINT ( 'NONE',  ( 5.000000000000000000, -26.00000000000000355, 0.000000000000000000 ) ) ;
#4003 = DIRECTION ( 'NONE',  ( 0.000000000000000000, 0.000000000000000000, -1.000000000000000000 ) ) ;
#4004 = CARTESIAN_POINT ( 'NONE',  ( -50.51988060489983212, 1.999999999999998224, 62.50099999999999767 ) ) ;
#4005 = CARTESIAN_POINT ( 'NONE',  ( -2.390265326283148806, -4.391654775818394363, -6.375000000000001776 ) ) ;
#4006 = CARTESIAN_POINT ( 'NONE',  ( 5.000000000000004441, 0.000000000000000000, 0.000000000000000000 ) ) ;
#4007 = EDGE_CURVE ( 'NONE', #2626, #7077, #14076, .T. ) ;
#4008 = CARTESIAN_POINT ( 'NONE',  ( -3.540020015735593439, -2.810662092924100630, -3.602146406945814672 ) ) ;
#4009 = EDGE_CURVE ( 'NONE', #8590, #9210, #592, .T. ) ;
#4010 = CARTESIAN_POINT ( 'NONE',  ( -4.458734124999999437, -22.93750000136559564, -5.460374474430324690E-16 ) ) ;
#4011 = CARTESIAN_POINT ( 'NONE',  ( 3.033343224707661712, -3.753672977998669946, -7.749999998634409692 ) ) ;
#4012 = ORIENTED_EDGE ( 'NONE', *, *, #14328, .T. ) ;
#4013 = DIRECTION ( 'NONE',  ( -0.000000000000000000, -1.000000000000000000, -0.000000000000000000 ) ) ;
#4014 = VERTEX_POINT ( 'NONE', #3003 ) ;
#4015 = ORIENTED_EDGE ( 'NONE', *, *, #13061, .F. ) ;
#4016 = AXIS2_PLACEMENT_3D ( 'NONE', #2171, #8417, #1279 ) ;
#4017 = VECTOR ( 'NONE', #1356, 1000.000000000000000 ) ;
#4019 = EDGE_CURVE ( 'NONE', #10675, #15938, #5597, .T. ) ;
#4018 = CARTESIAN_POINT ( 'NONE',  ( -8.190561711645485556E-16, -22.68750000136559564, 4.458734124999999437 ) ) ;
#4020 = CARTESIAN_POINT ( 'NONE',  ( 4.896370289181002811, 0.000000000000000000, -48.48076211353215825 ) ) ;
#4021 = ORIENTED_EDGE ( 'NONE', *, *, #2927, .T. ) ;
#4022 = CARTESIAN_POINT ( 'NONE',  ( 5.000000000000000888, 0.000000000000000000, -25.03750572909317285 ) ) ;
#4023 = CIRCLE ( 'NONE', #423, 2.649999999999992806 ) ;
#4024 = CARTESIAN_POINT ( 'NONE',  ( 0.6511518506208961998, -8.763486134561278007, -7.907570769506053310 ) ) ;
#4025 = CARTESIAN_POINT ( 'NONE',  ( 0.000000000000000000, -20.00000000000000000, 0.000000000000000000 ) ) ;
#4026 = LINE ( 'NONE', #2973, #9618 ) ;
#4027 = CARTESIAN_POINT ( 'NONE',  ( 3.535533905932738197, -28.87500000000000000, -3.535533905932738197 ) ) ;
#4028 = CIRCLE ( 'NONE', #12800, 60.00000000000000000 ) ;
#4029 = CARTESIAN_POINT ( 'NONE',  ( -2.805705207896067144, 3.226868319750155312, -3.503898532754364581 ) ) ;
#4030 = CARTESIAN_POINT ( 'NONE',  ( -67.50000000000000000, 50.00000000000000000, -7.070249711157346244E-13 ) ) ;
#4031 = ADVANCED_FACE ( 'NONE', ( #523 ), #5678, .T. ) ;
#4032 = CARTESIAN_POINT ( 'NONE',  ( 3.061616997868383141E-16, -22.87500000273118772, -5.000000000000000000 ) ) ;
#4033 = FACE_BOUND ( 'NONE', #11763, .T. ) ;
#4034 = CARTESIAN_POINT ( 'NONE',  ( 1.846868145590735200, -27.25000000136559564, -4.458734124999999437 ) ) ;
#4035 =( NAMED_UNIT ( * ) SI_UNIT ( $, .STERADIAN. ) SOLID_ANGLE_UNIT ( ) );
#4036 = VERTEX_POINT ( 'NONE', #10533 ) ;
#4037 = VECTOR ( 'NONE', #8113, 1000.000000000000000 ) ;
#4038 = ORIENTED_EDGE ( 'NONE', *, *, #3942, .T. ) ;
#4039 = ORIENTED_EDGE ( 'NONE', *, *, #3162, .T. ) ;
#4040 = CARTESIAN_POINT ( 'NONE',  ( -44.22043002422942948, -3.387975324183347237, 20.78776903885821881 ) ) ;
#4041 = CIRCLE ( 'NONE', #9713, 2.649999999999985700 ) ;
#4042 = VERTEX_POINT ( 'NONE', #8037 ) ;
#4043 = DIRECTION ( 'NONE',  ( 0.000000000000000000, 1.000000000000000000, 0.000000000000000000 ) ) ;
#4044 = AXIS2_PLACEMENT_3D ( 'NONE', #15755, #9591, #15826 ) ;
#4045 = DIRECTION ( 'NONE',  ( -0.000000000000000000, -1.000000000000000000, -0.000000000000000000 ) ) ;
#4046 = LINE ( 'NONE', #8917, #4614 ) ;
#4047 = DIRECTION ( 'NONE',  ( -1.000000000000000000, -0.000000000000000000, -0.000000000000000000 ) ) ;
#4048 = ADVANCED_FACE ( 'NONE', ( #7952 ), #2706, .F. ) ;
#4049 = EDGE_CURVE ( 'NONE', #2497, #4880, #7891, .T. ) ;
#4050 = PRODUCT_DEFINITION_FORMATION_WITH_SPECIFIED_SOURCE ( 'ANY', '', #873, .NOT_KNOWN. ) ;
#4051 = EDGE_CURVE ( 'NONE', #5600, #7177, #10162, .T. ) ;
#4052 = CONTEXT_DEPENDENT_SHAPE_REPRESENTATION ( #15497, #1761 ) ;
#4053 = CARTESIAN_POINT ( 'NONE',  ( 3.753672977998667726, 3.033343224707664376, -6.499999998634407916 ) ) ;
#4054 = DIRECTION ( 'NONE',  ( 0.000000000000000000, -1.000000000000000000, -2.775557561562892929E-15 ) ) ;
#4055 = ORIENTED_EDGE ( 'NONE', *, *, #7862, .T. ) ;
#4056 = CARTESIAN_POINT ( 'NONE',  ( 3.882512440569886980, -3.242827243955292094, -48.74656899134319588 ) ) ;
#4057 = ORIENTED_EDGE ( 'NONE', *, *, #3235, .F. ) ;
#4058 = CARTESIAN_POINT ( 'NONE',  ( -5.000000000000092371, -0.7223674278660636716, -7.521799365517158442 ) ) ;
#4059 = CIRCLE ( 'NONE', #2246, 5.000000000000000000 ) ;
#4060 = DIRECTION ( 'NONE',  ( 0.000000000000000000, 0.000000000000000000, 1.000000000000000000 ) ) ;
#4061 = VERTEX_POINT ( 'NONE', #15002 ) ;
#4062 = CONTEXT_DEPENDENT_SHAPE_REPRESENTATION ( #15798, #15146 ) ;
#4063 = CARTESIAN_POINT ( 'NONE',  ( 3.033343224707661712, -3.753672977998669502, -7.749999998634409692 ) ) ;
#4064 = AXIS2_PLACEMENT_3D ( 'NONE', #3673, #9533, #2535 ) ;
#4065 = FACE_OUTER_BOUND ( 'NONE', #7295, .T. ) ;
#4066 = CARTESIAN_POINT ( 'NONE',  ( -6.259644161404860030E-16, -4.618802153517027165, -5.000000000000000000 ) ) ;
#4067 = VECTOR ( 'NONE', #14769, 1000.000000000000114 ) ;
#4068 = CARTESIAN_POINT ( 'NONE',  ( 2.500000000000000000, 2.357898499370433054, -1.951563910473907981E-15 ) ) ;
#4069 = ADVANCED_FACE ( 'NONE', ( #3915, #9101 ), #1501, .F. ) ;
#4070 = CARTESIAN_POINT ( 'NONE',  ( 3.401574460001763001, -4.209348295687703967, -2.062499997268814500 ) ) ;
#4071 = FACE_OUTER_BOUND ( 'NONE', #6484, .T. ) ;
#4072 = CARTESIAN_POINT ( 'NONE',  ( -4.468245232710503778, 1.275674966182978265, -0.2551639277954672602 ) ) ;
#4073 = LINE ( 'NONE', #13763, #3983 ) ;
#4074 = ORIENTED_EDGE ( 'NONE', *, *, #10083, .F. ) ;
#4075 = CARTESIAN_POINT ( 'NONE',  ( -2.886751345948139758, -4.999999999999997335, 35.00000000000000000 ) ) ;
#4076 = CARTESIAN_POINT ( 'NONE',  ( -4.799145180956616130, 0.5093500532425063732, -6.874999998634407916 ) ) ;
#4077 = VECTOR ( 'NONE', #7383, 1000.000000000000000 ) ;
#4078 = CARTESIAN_POINT ( 'NONE',  ( -5.725490332117410652, -3.000000000000000000, 9.916840153471811803 ) ) ;
#4079 = ORIENTED_EDGE ( 'NONE', *, *, #12282, .T. ) ;
#4080 = ORIENTED_EDGE ( 'NONE', *, *, #14643, .T. ) ;
#4081 =( BOUNDED_CURVE ( )  B_SPLINE_CURVE ( 2, ( #12308, #14918, #7568, #50, #9979, #12465, #2695, #12630, #217 ),
 .UNSPECIFIED., .F., .F. ) 
 B_SPLINE_CURVE_WITH_KNOTS ( ( 3, 2, 2, 2, 3 ),
 ( 0.2749999999999999112, 0.2874999999999998668, 0.2999999999999999334, 0.3124999999999999445, 0.3249999999999999556 ),
 .UNSPECIFIED. ) 
 CURVE ( )  GEOMETRIC_REPRESENTATION_ITEM ( )  RATIONAL_B_SPLINE_CURVE ( ( 1.000000000000000666, 0.9238795325112860723, 1.000000000000000000, 0.9238795325112867385, 1.000000000000000000, 0.9238795325112867385, 1.000000000000000000, 0.9238795325112870716, 0.9999999999999996669 ) ) 
 REPRESENTATION_ITEM ( '' )  );
#4082 = ORIENTED_EDGE ( 'NONE', *, *, #13038, .T. ) ;
#4083 = CARTESIAN_POINT ( 'NONE',  ( -3.288228914120471913, 7.217643567644807412, -7.591235721156636806 ) ) ;
#4084 = MECHANICAL_DESIGN_GEOMETRIC_PRESENTATION_REPRESENTATION (  '', ( #11057 ), #13887 ) ;
#4085 = CARTESIAN_POINT ( 'NONE',  ( -45.00000000000000000, 0.000000000000000000, -7.500000000000000000 ) ) ;
#4086 = AXIS2_PLACEMENT_3D ( 'NONE', #8210, #9633, #8367 ) ;
#4087 = DIRECTION ( 'NONE',  ( 0.000000000000000000, 0.000000000000000000, 1.000000000000000000 ) ) ;
#4088 =( GEOMETRIC_REPRESENTATION_CONTEXT ( 3 ) GLOBAL_UNCERTAINTY_ASSIGNED_CONTEXT ( ( #9358 ) ) GLOBAL_UNIT_ASSIGNED_CONTEXT ( ( #13509, #7319, #12307 ) ) REPRESENTATION_CONTEXT ( 'NONE', 'WORKASPACE' ) );
#4089 = CARTESIAN_POINT ( 'NONE',  ( 35.00000000000000000, 37.00000000000000000, 5.999999999999991118 ) ) ;
#4090 = DIRECTION ( 'NONE',  ( 0.000000000000000000, 0.000000000000000000, -1.000000000000000000 ) ) ;
#4091 = DIRECTION ( 'NONE',  ( -0.8660254037844383745, 0.000000000000000000, -0.5000000000000006661 ) ) ;
#4092 = CARTESIAN_POINT ( 'NONE',  ( -0.5711823568785978633, -5.381735091635035495, -5.312499999999999112 ) ) ;
#4093 = DIRECTION ( 'NONE',  ( 1.000000000000000000, 0.000000000000000000, 0.000000000000000000 ) ) ;
#4094 = CIRCLE ( 'NONE', #6171, 5.999999999999991118 ) ;
#4095 = CARTESIAN_POINT ( 'NONE',  ( -2.836893136758495970, -3.208949435745868328, -3.505054077164885484 ) ) ;
#4096 = CARTESIAN_POINT ( 'NONE',  ( 12.67949192431120586, -4.999999999999997335, 61.96152422706632024 ) ) ;
#4097 = AXIS2_PLACEMENT_3D ( 'NONE', #11691, #4188, #1838 ) ;
#4098 = CARTESIAN_POINT ( 'NONE',  ( -3.033343224707664376, 3.753672977998667726, -5.249999998634407028 ) ) ;
#4099 = ORIENTED_EDGE ( 'NONE', *, *, #1782, .T. ) ;
#4100 = CARTESIAN_POINT ( 'NONE',  ( 0.000000000000000000, -11.00000000000000178, 0.000000000000000000 ) ) ;
#4101 = VERTEX_POINT ( 'NONE', #8943 ) ;
#4102 = ORIENTED_EDGE ( 'NONE', *, *, #6738, .F. ) ;
#4103 = ORIENTED_EDGE ( 'NONE', *, *, #9313, .F. ) ;
#4104 = CARTESIAN_POINT ( 'NONE',  ( 1.846868145590736310, -29.87500000136559564, 4.458734124999999437 ) ) ;
#4105 = CARTESIAN_POINT ( 'NONE',  ( -7.922281120364393914, -4.573931137438277617, -8.047472243342932430 ) ) ;
#4106 = ORIENTED_EDGE ( 'NONE', *, *, #226, .F. ) ;
#4107 = DIRECTION ( 'NONE',  ( 1.000000000000000000, 0.000000000000000000, 0.000000000000000000 ) ) ;
#4108 = EDGE_CURVE ( 'NONE', #637, #1925, #2830, .T. ) ;
#4109 = EDGE_CURVE ( 'NONE', #11530, #15795, #2859, .T. ) ;
#4110 = CIRCLE ( 'NONE', #5926, 57.99999999999999289 ) ;
#4111 = DIRECTION ( 'NONE',  ( 0.000000000000000000, 0.8660254037844380415, -0.5000000000000011102 ) ) ;
#4112 = CARTESIAN_POINT ( 'NONE',  ( 4.420982230657666712, -0.5789871446316176007, -0.3789984458506777676 ) ) ;
#4113 = DIRECTION ( 'NONE',  ( 0.000000000000000000, 0.000000000000000000, 1.000000000000000000 ) ) ;
#4114 = CARTESIAN_POINT ( 'NONE',  ( 2.071067811865476394, -31.18750000000000355, 5.000000000000000000 ) ) ;
#4115 = CARTESIAN_POINT ( 'NONE',  ( -3.753672977998669946, -3.033343224707661712, -4.749999998634407028 ) ) ;
#4116 = CARTESIAN_POINT ( 'NONE',  ( -44.12168325659714441, -3.194220869028276066, -21.13058177393697434 ) ) ;
#4117 = CARTESIAN_POINT ( 'NONE',  ( 3.061616997868383141E-16, -26.75000000000000000, -5.000000000000000000 ) ) ;
#4118 = CARTESIAN_POINT ( 'NONE',  ( -3.535533905932738641, -22.50000000273118772, 3.535533905932737309 ) ) ;
#4119 = CARTESIAN_POINT ( 'NONE',  ( 42.02221399786069611, -3.000000000000001332, 1.040834085586084257E-13 ) ) ;
#4120 = CARTESIAN_POINT ( 'NONE',  ( 4.458734124999999437, -27.37500000136559564, -1.846868145590734978 ) ) ;
#4121 = FACE_OUTER_BOUND ( 'NONE', #8533, .T. ) ;
#4122 = ORIENTED_EDGE ( 'NONE', *, *, #4947, .F. ) ;
#4123 = ORIENTED_EDGE ( 'NONE', *, *, #2152, .T. ) ;
#4124 = EDGE_LOOP ( 'NONE', ( #9267, #6242, #15766 ) ) ;
#4125 = CARTESIAN_POINT ( 'NONE',  ( 10.00000000000098765, -20.00000000000000000, 17.32050807568871065 ) ) ;
#4126 = EDGE_LOOP ( 'NONE', ( #598, #10600, #4186, #11155 ) ) ;
#4127 = FACE_OUTER_BOUND ( 'NONE', #6244, .T. ) ;
#4128 = ADVANCED_FACE ( 'NONE', ( #6681 ), #456, .T. ) ;
#4129 = EDGE_CURVE ( 'NONE', #8026, #6165, #9491, .T. ) ;
#4130 =( REPRESENTATION_RELATIONSHIP ('NONE','NONE', #4176, #15130 ) REPRESENTATION_RELATIONSHIP_WITH_TRANSFORMATION ( #6655 )SHAPE_REPRESENTATION_RELATIONSHIP( ) );
#4131 = CARTESIAN_POINT ( 'NONE',  ( 7.922281120364393914, 4.573931137438269623, -8.047472243342932430 ) ) ;
#4132 = CARTESIAN_POINT ( 'NONE',  ( 4.458734124999999437, -31.68750000136559564, 0.000000000000000000 ) ) ;
#4133 = DIRECTION ( 'NONE',  ( -0.000000000000000000, -1.000000000000000000, -0.000000000000000000 ) ) ;
#4134 = CARTESIAN_POINT ( 'NONE',  ( 0.000000000000000000, 1.178949249685218525, 2.041999999999999371 ) ) ;
#4135 = CARTESIAN_POINT ( 'NONE',  ( 4.799145180956616130, -0.5093500532425063732, 0.3750000013655915843 ) ) ;
#4136 = VERTEX_POINT ( 'NONE', #14422 ) ;
#4137 = SURFACE_STYLE_USAGE ( .BOTH. , #13991 ) ;
#4138 = EDGE_LOOP ( 'NONE', ( #9106, #15622, #4269, #3027, #3558 ) ) ;
#4139 = PLANE ( 'NONE',  #3591 ) ;
#4140 = CARTESIAN_POINT ( 'NONE',  ( -28.86751345948129455, 0.000000000000000000, 49.99999999999999289 ) ) ;
#4141 = ORIENTED_EDGE ( 'NONE', *, *, #4746, .T. ) ;
#4142 = CARTESIAN_POINT ( 'NONE',  ( -3.033343224707664820, 3.753672977998667726, -5.249999998634407916 ) ) ;
#4143 = EDGE_CURVE ( 'NONE', #2071, #14412, #180, .T. ) ;
#4144 = EDGE_CURVE ( 'NONE', #7386, #12557, #1969, .T. ) ;
#4145 =( NAMED_UNIT ( * ) PLANE_ANGLE_UNIT ( ) SI_UNIT ( $, .RADIAN. ) );
#4146 = DIRECTION ( 'NONE',  ( 1.000000000000000000, 1.734723475976808080E-16, 0.000000000000000000 ) ) ;
#4147 = CARTESIAN_POINT ( 'NONE',  ( -5.000000000000002665, -1.404940523648820476E-14, -8.420263044861757251 ) ) ;
#4148 = PRODUCT_DEFINITION_CONTEXT ( 'detailed design', #2780, 'design' ) ;
#4149 = CARTESIAN_POINT ( 'NONE',  ( 1.415196051561583790, -4.795541693661363958, -8.124999997268814056 ) ) ;
#4150 = CARTESIAN_POINT ( 'NONE',  ( -5.000000000000000888, -23.43749999999999645, 2.071067811865474617 ) ) ;
#4151 = CARTESIAN_POINT ( 'NONE',  ( -60.00000000000000000, 88.59290746114278647, -18.00000000000001066 ) ) ;
#4152 = CARTESIAN_POINT ( 'NONE',  ( 3.152801135295367541, -22.56250000136559564, -3.152801135295367541 ) ) ;
#4153 = ORIENTED_EDGE ( 'NONE', *, *, #15197, .T. ) ;
#4154 = CARTESIAN_POINT ( 'NONE',  ( 2.143131898507869826E-15, 37.00000000000000000, -67.50000000000000000 ) ) ;
#4155 = CARTESIAN_POINT ( 'NONE',  ( -31.74999999999995737, 0.000000000000000000, 2.500000000000000444 ) ) ;
#4156 = FACE_BOUND ( 'NONE', #2166, .T. ) ;
#4157 = ORIENTED_EDGE ( 'NONE', *, *, #4658, .F. ) ;
#4158 = CARTESIAN_POINT ( 'NONE',  ( -4.000000000000000000, 1.700094919196744270, -3.320312364301766017 ) ) ;
#4159 = ORIENTED_EDGE ( 'NONE', *, *, #12723, .F. ) ;
#4160 = ORIENTED_EDGE ( 'NONE', *, *, #5940, .T. ) ;
#4161 = FACE_OUTER_BOUND ( 'NONE', #10744, .T. ) ;
#4162 = EDGE_CURVE ( 'NONE', #3541, #7075, #13604, .T. ) ;
#4163 = CARTESIAN_POINT ( 'NONE',  ( 0.1750025118121568690, 4.719839900820621104, -3.469254087858248070 ) ) ;
#4164 = EDGE_CURVE ( 'NONE', #10322, #8883, #15401, .T. ) ;
#4165 = CARTESIAN_POINT ( 'NONE',  ( -5.047120108843201614, 5.746297884371392328, -0.1007566405101798096 ) ) ;
#4166 = CARTESIAN_POINT ( 'NONE',  ( -9.184850993605147944E-16, -26.37500000273118417, 5.000000000000000000 ) ) ;
#4167 = DIRECTION ( 'NONE',  ( -0.000000000000000000, -1.000000000000000000, -0.000000000000000000 ) ) ;
#4168 = CARTESIAN_POINT ( 'NONE',  ( 14.41154273188013590, -5.000000000000000000, -60.96152422706632024 ) ) ;
#4169 = PRODUCT_DEFINITION_SHAPE ( 'NONE', 'NONE',  #15977 ) ;
#4170 = CARTESIAN_POINT ( 'NONE',  ( -4.209348295687703967, -3.401574460001763001, -4.437500000000000888 ) ) ;
#4171 = CARTESIAN_POINT ( 'NONE',  ( -4.999999999999849898, 1.272547481429008309, -2.586597482644648949 ) ) ;
#4172 = VECTOR ( 'NONE', #2179, 1000.000000000000000 ) ;
#4173 = CARTESIAN_POINT ( 'NONE',  ( 5.000000000000000000, -25.12500000273118417, 0.000000000000000000 ) ) ;
#4174 = CARTESIAN_POINT ( 'NONE',  ( -4.458734125000000326, -23.00000000136559564, -1.846868145590735644 ) ) ;
#4175 =( BOUNDED_SURFACE ( )  B_SPLINE_SURFACE ( 3, 2, ( 
 ( #4286, #11701, #8020 ),
 ( #15452, #11627, #3152 ),
 ( #13972, #10429, #12751 ),
 ( #15364, #4373, #1696 ),
 ( #8097, #1928, #505 ),
 ( #5662, #10602, #2827 ),
 ( #15284, #5425, #13301 ),
 ( #5973, #14302, #6050 ) ),
 .UNSPECIFIED., .F., .F., .F. ) 
 B_SPLINE_SURFACE_WITH_KNOTS ( ( 4, 2, 2, 4 ),
 ( 3, 3 ),
 ( 0.03861844051980971304, 0.04325213341840643266, 0.04556897986770479247, 0.04788582631700314535 ),
 ( 0.000000000000000000, 1.000000000000000000 ),
 .UNSPECIFIED. ) 
 GEOMETRIC_REPRESENTATION_ITEM ( )  RATIONAL_B_SPLINE_SURFACE ( (
 ( 1.000000000000000000, 0.8047781759831919013, 1.000000000000000000),
 ( 1.000000000000000000, 0.8123762462801796813, 1.000000000000000000),
 ( 1.000000000000000000, 0.8190659850621079263, 1.000000000000000000),
 ( 1.000000000000000000, 0.8191937571011467245, 1.000000000000000000),
 ( 1.000000000000000000, 0.8176092952778544198, 1.000000000000000000),
 ( 1.000000000000000000, 0.8122962088598406627, 1.000000000000000000),
 ( 1.000000000000000000, 0.8086311330826504440, 1.000000000000000000),
 ( 1.000000000000000000, 0.8047712282214325441, 1.000000000000000000) ) ) 
 REPRESENTATION_ITEM ( '' )  SURFACE ( )  );
#4176 = SHAPE_REPRESENTATION ( 'BR-003', ( #15939, #5276, #10190, #13507, #1659, #2692, #1401, #14313, #6054, #7349, #14827, #12493, #7874, #14568, #385, #9661, #4769, #2420, #6573, #9921, #6842, #11467, #2947, #4504, #14056, #1926, #7101, #125, #15612, #9165, #8645, #11215, #4246, #13259, #10452, #15873, #957 ), #11277 ) ;
#4177 = CARTESIAN_POINT ( 'NONE',  ( -0.5093500532425060401, -4.799145180956616130, -4.874999998634405252 ) ) ;
#4178 = ORIENTED_EDGE ( 'NONE', *, *, #13550, .F. ) ;
#4179 = UNCERTAINTY_MEASURE_WITH_UNIT (LENGTH_MEASURE( 1.000000000000000082E-05 ), #14586, 'distance_accuracy_value', 'NONE');
#4180 = CARTESIAN_POINT ( 'NONE',  ( 24.55500000000002103, 0.000000000000000000, 2.500000000000001332 ) ) ;
#4181 = ORIENTED_EDGE ( 'NONE', *, *, #8556, .T. ) ;
#4182 = ORIENTED_EDGE ( 'NONE', *, *, #11259, .F. ) ;
#4183 = CARTESIAN_POINT ( 'NONE',  ( 4.458734125000000326, -31.62500000136559564, -1.846868145590734978 ) ) ;
#4184 = CARTESIAN_POINT ( 'NONE',  ( -2.804994570502171047, -3.229033611042465335, -3.526374918436838701 ) ) ;
#4185 = EDGE_CURVE ( 'NONE', #12880, #15286, #1454, .T. ) ;
#4186 = ORIENTED_EDGE ( 'NONE', *, *, #9806, .T. ) ;
#4187 = DIRECTION ( 'NONE',  ( 0.000000000000000000, 0.000000000000000000, -1.000000000000000000 ) ) ;
#4188 = DIRECTION ( 'NONE',  ( -0.000000000000000000, -1.000000000000000000, -0.000000000000000000 ) ) ;
#4189 = CARTESIAN_POINT ( 'NONE',  ( 4.458734124999999437, -21.68750000136559208, 0.000000000000000000 ) ) ;
#4190 = PLANE ( 'NONE',  #4721 ) ;
#4191 = CARTESIAN_POINT ( 'NONE',  ( -2.071067811865475061, -25.68750000000000355, -5.000000000000000888 ) ) ;
#4192 = CARTESIAN_POINT ( 'NONE',  ( -4.276409079477644148, -1.261996585732578335, -4.812499998634405252 ) ) ;
#4193 = CARTESIAN_POINT ( 'NONE',  ( -1.250000000000000444, -7.938566201357371455, -7.198902722707432922 ) ) ;
#4194 = CARTESIAN_POINT ( 'NONE',  ( 35.00000000000000000, 37.00000000000000000, 2.649999999999983924 ) ) ;
#4195 = CARTESIAN_POINT ( 'NONE',  ( 5.000000000000000000, -23.12500000273118772, 0.000000000000000000 ) ) ;
#4196 = CARTESIAN_POINT ( 'NONE',  ( 3.401574460001763445, -4.209348295687703079, -3.187500000000003553 ) ) ;
#4197 = CARTESIAN_POINT ( 'NONE',  ( -4.458734124999999437, -25.93750000136559564, -5.460374474430324690E-16 ) ) ;
#4198 = EDGE_CURVE ( 'NONE', #15286, #10806, #9264, .T. ) ;
#4199 = CARTESIAN_POINT ( 'NONE',  ( -3.401574460001765221, 4.209348295687701302, -6.687500000000003553 ) ) ;
#4200 = EDGE_LOOP ( 'NONE', ( #13482, #6376, #13438, #14194, #1217 ) ) ;
#4201 = EDGE_LOOP ( 'NONE', ( #12815, #7497, #12056, #14443 ) ) ;
#4202 = CARTESIAN_POINT ( 'NONE',  ( -28.86751345948126612, 88.59290746114278647, -18.00000000000000355 ) ) ;
#4203 = ORIENTED_EDGE ( 'NONE', *, *, #15548, .T. ) ;
#4204 = CIRCLE ( 'NONE', #2907, 5.000000000000000000 ) ;
#4205 = DIRECTION ( 'NONE',  ( 0.000000000000000000, 0.000000000000000000, 1.000000000000000000 ) ) ;
#4206 = ORIENTED_EDGE ( 'NONE', *, *, #9325, .T. ) ;
#4207 = DIRECTION ( 'NONE',  ( -0.000000000000000000, 1.000000000000000000, -0.000000000000000000 ) ) ;
#4208 = PRODUCT ( 'Drive Unit', 'Drive Unit', '', ( #11715 ) ) ;
#4209 = CARTESIAN_POINT ( 'NONE',  ( -50.51988060489983212, 1.999999999999998224, 62.50099999999999767 ) ) ;
#4210 = CARTESIAN_POINT ( 'NONE',  ( -3.152801135295367985, -28.06250000136559564, 3.152801135295367096 ) ) ;
#4211 = CIRCLE ( 'NONE', #2137, 2.041999999999999815 ) ;
#4212 = CARTESIAN_POINT ( 'NONE',  ( 6.123233995736766282E-16, -13.00000000000000178, 5.000000000000000000 ) ) ;
#4213 = ITEM_DEFINED_TRANSFORMATION ( 'NONE', 'NONE', #14313,  #3223 ) ;
#4214 = CARTESIAN_POINT ( 'NONE',  ( 3.750000000000001776, -6.495190528383298911, -6.991905250253755533 ) ) ;
#4215 = DIRECTION ( 'NONE',  ( 0.000000000000000000, 0.000000000000000000, 1.000000000000000000 ) ) ;
#4216 = EDGE_CURVE ( 'NONE', #5811, #6058, #8132, .T. ) ;
#4218 = EDGE_CURVE ( 'NONE', #15077, #11474, #9709, .T. ) ;
#4217 = ORIENTED_EDGE ( 'NONE', *, *, #1259, .T. ) ;
#4219 = VERTEX_POINT ( 'NONE', #4478 ) ;
#4220 = DIRECTION ( 'NONE',  ( -0.9999824063907751803, -0.005931855436079011210, 0.000000000000000000 ) ) ;
#4221 = CARTESIAN_POINT ( 'NONE',  ( 3.152801135295367541, -28.31250000136559564, -3.152801135295367541 ) ) ;
#4222 = ORIENTED_EDGE ( 'NONE', *, *, #11352, .T. ) ;
#4223 = CONTEXT_DEPENDENT_SHAPE_REPRESENTATION ( #9401, #3904 ) ;
#4224 = AXIS2_PLACEMENT_3D ( 'NONE', #8780, #9025, #4229 ) ;
#4225 = CARTESIAN_POINT ( 'NONE',  ( 42.02221399786069611, 2.000000000000000000, 1.075528555105620399E-13 ) ) ;
#4226 = CARTESIAN_POINT ( 'NONE',  ( 0.000000000000000000, -13.00000000000000178, 0.000000000000000000 ) ) ;
#4227 = FACE_OUTER_BOUND ( 'NONE', #10200, .T. ) ;
#4228 = CARTESIAN_POINT ( 'NONE',  ( 4.391654775818395251, -2.390265326283149694, -5.999999997268814944 ) ) ;
#4229 = DIRECTION ( 'NONE',  ( 0.000000000000000000, 0.000000000000000000, 1.000000000000000000 ) ) ;
#4230 = ADVANCED_FACE ( 'NONE', ( #1888, #6829 ), #772, .T. ) ;
#4231 = CARTESIAN_POINT ( 'NONE',  ( -5.000000000000004441, -7.530481206757679743E-15, -1.545263047592943861 ) ) ;
#4232 = DIRECTION ( 'NONE',  ( -0.000000000000000000, 1.000000000000000000, -0.000000000000000000 ) ) ;
#4233 = EDGE_CURVE ( 'NONE', #513, #9050, #1061, .T. ) ;
#4234 = EDGE_LOOP ( 'NONE', ( #15251, #1543, #9230, #14107, #6886 ) ) ;
#4235 = DIRECTION ( 'NONE',  ( 0.000000000000000000, 0.000000000000000000, -1.000000000000000000 ) ) ;
#4236 = CARTESIAN_POINT ( 'NONE',  ( 3.033343224707661712, -3.753672977998669946, -6.499999998634407916 ) ) ;
#4237 = DIRECTION ( 'NONE',  ( -0.000000000000000000, 1.000000000000000000, -0.000000000000000000 ) ) ;
#4238 = ORIENTED_EDGE ( 'NONE', *, *, #5340, .T. ) ;
#4239 = CARTESIAN_POINT ( 'NONE',  ( -4.000000000000000000, 2.511478553582031203, -3.469254451724764543 ) ) ;
#4240 = VERTEX_POINT ( 'NONE', #2052 ) ;
#4241 = AXIS2_PLACEMENT_3D ( 'NONE', #12986, #806, #1922 ) ;
#4242 = ORIENTED_EDGE ( 'NONE', *, *, #13940, .F. ) ;
#4243 = FACE_OUTER_BOUND ( 'NONE', #6518, .T. ) ;
#4244 = DIRECTION ( 'NONE',  ( -0.000000000000000000, -0.000000000000000000, 1.000000000000000000 ) ) ;
#4245 = DIRECTION ( 'NONE',  ( 0.8660254037844407060, -0.4999999999999965583, 0.000000000000000000 ) ) ;
#4246 = AXIS2_PLACEMENT_3D ( 'NONE', #12446, #12524, #1469 ) ;
#4247 = DIRECTION ( 'NONE',  ( 0.000000000000000000, 0.000000000000000000, 1.000000000000000000 ) ) ;
#4248 = DIRECTION ( 'NONE',  ( 0.000000000000000000, 0.000000000000000000, 1.000000000000000000 ) ) ;
#4249 = AXIS2_PLACEMENT_3D ( 'NONE', #14349, #14271, #9112 ) ;
#4250 = CARTESIAN_POINT ( 'NONE',  ( 3.061616997868383141E-16, -22.75000000000000000, -5.000000000000000000 ) ) ;
#4251 = LINE ( 'NONE', #9198, #7166 ) ;
#4252 = LINE ( 'NONE', #1825, #8364 ) ;
#4253 = EDGE_CURVE ( 'NONE', #2121, #1994, #11052, .T. ) ;
#4254 = CARTESIAN_POINT ( 'NONE',  ( 27.50000000000003197, -5.000000000000000000, -47.63139720814412925 ) ) ;
#4255 = EDGE_CURVE ( 'NONE', #13119, #10556, #13568, .T. ) ;
#4256 = CARTESIAN_POINT ( 'NONE',  ( -1.846868145590737420, -22.75000000136559208, 4.458734124999999437 ) ) ;
#4257 = EDGE_CURVE ( 'NONE', #5955, #4331, #5854, .T. ) ;
#4258 = CARTESIAN_POINT ( 'NONE',  ( 2.131511515620586383, 3.916244202832140253, -8.437499998634409692 ) ) ;
#4259 = ORIENTED_EDGE ( 'NONE', *, *, #186, .F. ) ;
#4260 = FACE_OUTER_BOUND ( 'NONE', #10880, .T. ) ;
#4261 = ORIENTED_EDGE ( 'NONE', *, *, #8019, .T. ) ;
#4262 = ORIENTED_EDGE ( 'NONE', *, *, #10365, .T. ) ;
#4263 = AXIS2_PLACEMENT_3D ( 'NONE', #618, #2937, #2860 ) ;
#4265 = VECTOR ( 'NONE', #11818, 1000.000000000000000 ) ;
#4264 = SURFACE_STYLE_FILL_AREA ( #7536 ) ;
#4266 = CARTESIAN_POINT ( 'NONE',  ( -8.190561711645485556E-16, -29.93750000136559564, 4.458734124999999437 ) ) ;
#4267 = CARTESIAN_POINT ( 'NONE',  ( -5.000000000000002665, -1.404940523648820476E-14, -7.545263047592946748 ) ) ;
#4268 =( GEOMETRIC_REPRESENTATION_CONTEXT ( 3 ) GLOBAL_UNCERTAINTY_ASSIGNED_CONTEXT ( ( #11761 ) ) GLOBAL_UNIT_ASSIGNED_CONTEXT ( ( #13754, #11343, #3979 ) ) REPRESENTATION_CONTEXT ( 'NONE', 'WORKASPACE' ) );
#4269 = ORIENTED_EDGE ( 'NONE', *, *, #5223, .T. ) ;
#4270 = DIRECTION ( 'NONE',  ( 0.000000000000000000, 1.000000000000000000, 0.000000000000000000 ) ) ;
#4271 = CARTESIAN_POINT ( 'NONE',  ( 7.500000000000346390, 1.545478204151935930, -7.491761935629074109 ) ) ;
#4272 = CARTESIAN_POINT ( 'NONE',  ( -3.033343224707664820, 3.753672977998667726, -3.999999998634406584 ) ) ;
#4273 = CARTESIAN_POINT ( 'NONE',  ( -4.999999999999844569, 1.272547481429019856, -5.461597479913463893 ) ) ;
#4274 =( BOUNDED_CURVE ( )  B_SPLINE_CURVE ( 3, ( #10885, #9832, #14765, #5965 ),
 .UNSPECIFIED., .F., .F. ) 
 B_SPLINE_CURVE_WITH_KNOTS ( ( 4, 4 ),
 ( 1.570796326794898334, 3.141592653589793116 ),
 .UNSPECIFIED. ) 
 CURVE ( )  GEOMETRIC_REPRESENTATION_ITEM ( )  RATIONAL_B_SPLINE_CURVE ( ( 1.000000000000000000, 0.8047378541243654926, 0.8047378541243654926, 1.000000000000000000 ) ) 
 REPRESENTATION_ITEM ( '' )  );
#4275 = CARTESIAN_POINT ( 'NONE',  ( 5.000000000000000000, -25.06250000000000355, 2.071067811865478614 ) ) ;
#4276 = CIRCLE ( 'NONE', #5302, 0.2000000000000000944 ) ;
#4277 = CARTESIAN_POINT ( 'NONE',  ( 3.401574460001763001, -4.209348295687703967, 1.812499999999996669 ) ) ;
#4278 = CARTESIAN_POINT ( 'NONE',  ( -43.85680617778868395, -3.000000000000000000, -22.00000000000000355 ) ) ;
#4279 = DIRECTION ( 'NONE',  ( 8.673617379884035472E-16, 0.000000000000000000, 1.000000000000000000 ) ) ;
#4280 = CARTESIAN_POINT ( 'NONE',  ( -5.000000000000000888, -25.56250000273118417, 2.071067811865474617 ) ) ;
#4281 = AXIS2_PLACEMENT_3D ( 'NONE', #9847, #13544, #11139 ) ;
#4282 = EDGE_CURVE ( 'NONE', #14880, #10728, #7157, .T. ) ;
#4283 = ORIENTED_EDGE ( 'NONE', *, *, #9373, .T. ) ;
#4284 = VECTOR ( 'NONE', #4270, 1000.000000000000000 ) ;
#4285 = CARTESIAN_POINT ( 'NONE',  ( 4.458734124999997661, -26.50000000136559564, 1.846868145590737864 ) ) ;
#4286 = CARTESIAN_POINT ( 'NONE',  ( -0.3470952277635217520, -8.860649561028104415, -7.493596212620246888 ) ) ;
#4287 = EDGE_LOOP ( 'NONE', ( #2697, #4153, #3535, #4754 ) ) ;
#4288 = ORIENTED_EDGE ( 'NONE', *, *, #4893, .T. ) ;
#4289 = FACE_OUTER_BOUND ( 'NONE', #4234, .T. ) ;
#4290 = EDGE_LOOP ( 'NONE', ( #12529, #95, #5463 ) ) ;
#4291 = CARTESIAN_POINT ( 'NONE',  ( 3.535533905932738197, -29.00000000273118772, -3.535533905932738197 ) ) ;
#4292 = ORIENTED_EDGE ( 'NONE', *, *, #3102, .T. ) ;
#4293 = ADVANCED_FACE ( 'NONE', ( #3375 ), #11123, .F. ) ;
#4294 = CARTESIAN_POINT ( 'NONE',  ( 0.000000000000000000, 0.000000000000000000, 0.000000000000000000 ) ) ;
#4295 = VECTOR ( 'NONE', #14216, 1000.000000000000000 ) ;
#4296 = EDGE_CURVE ( 'NONE', #13728, #15071, #11518, .T. ) ;
#4297 = CARTESIAN_POINT ( 'NONE',  ( 3.061616997868383141E-16, -31.75000000000000000, -5.000000000000000000 ) ) ;
#4298 = CARTESIAN_POINT ( 'NONE',  ( -8.190561711645485556E-16, -27.93750000136559564, 4.458734124999999437 ) ) ;
#4299 = CARTESIAN_POINT ( 'NONE',  ( 5.000000000000091482, 0.7223674278660666692, -0.8967993627859682793 ) ) ;
#4300 = CARTESIAN_POINT ( 'NONE',  ( 3.401574460001763445, -4.209348295687703079, -4.187500000000000888 ) ) ;
#4301 = SHAPE_DEFINITION_REPRESENTATION ( #8246, #6981 ) ;
#4302 = DIRECTION ( 'NONE',  ( -1.000000000000000000, -1.541976423090495140E-16, 0.000000000000000000 ) ) ;
#4303 = CARTESIAN_POINT ( 'NONE',  ( 0.2500000000000002220, 0.000000000000000000, 0.000000000000000000 ) ) ;
#4304 = EDGE_LOOP ( 'NONE', ( #12767, #3208, #12532, #11298 ) ) ;
#4305 =( NAMED_UNIT ( * ) PLANE_ANGLE_UNIT ( ) SI_UNIT ( $, .RADIAN. ) );
#4306 = ORIENTED_EDGE ( 'NONE', *, *, #14944, .T. ) ;
#4307 = CARTESIAN_POINT ( 'NONE',  ( -7.848314987057863235, 4.129027267381583322, -7.493854785173818200 ) ) ;
#4308 = ORIENTED_EDGE ( 'NONE', *, *, #6079, .F. ) ;
#4309 = VECTOR ( 'NONE', #13445, 1000.000000000000000 ) ;
#4310 =( NAMED_UNIT ( * ) SI_UNIT ( $, .STERADIAN. ) SOLID_ANGLE_UNIT ( ) );
#4311 = ORIENTED_EDGE ( 'NONE', *, *, #13694, .T. ) ;
#4312 = EDGE_CURVE ( 'NONE', #11044, #8136, #2155, .T. ) ;
#4313 = EDGE_CURVE ( 'NONE', #5426, #11703, #441, .T. ) ;
#4314 = DIRECTION ( 'NONE',  ( 1.000000000000000000, 0.000000000000000000, 0.000000000000000000 ) ) ;
#4315 = AXIS2_PLACEMENT_3D ( 'NONE', #2751, #11475, #425 ) ;
#4316 = CARTESIAN_POINT ( 'NONE',  ( 11.45098066423670247, -3.000000000000000000, 1.122567565269603304E-11 ) ) ;
#4317 = CARTESIAN_POINT ( 'NONE',  ( -4.000000000000000000, 0.000000000000000000, 0.000000000000000000 ) ) ;
#4318 = CARTESIAN_POINT ( 'NONE',  ( -3.033343224707664376, 3.753672977998667726, 0.7500000013655939712 ) ) ;
#4319 = DIRECTION ( 'NONE',  ( -0.000000000000000000, -1.000000000000000000, -0.000000000000000000 ) ) ;
#4320 = AXIS2_PLACEMENT_3D ( 'NONE', #15738, #13357, #7315 ) ;
#4321 = CARTESIAN_POINT ( 'NONE',  ( -3.401574460001765221, 4.209348295687701302, -1.687500000000002442 ) ) ;
#4322 = PLANE ( 'NONE',  #14068 ) ;
#4323 = ORIENTED_EDGE ( 'NONE', *, *, #15530, .T. ) ;
#4324 = DIRECTION ( 'NONE',  ( 0.000000000000000000, 0.000000000000000000, 1.000000000000000000 ) ) ;
#4325 = CARTESIAN_POINT ( 'NONE',  ( -7.808218555861950350, 4.508077085120202554, -7.999534413642741093 ) ) ;
#4326 = CARTESIAN_POINT ( 'NONE',  ( -1.154700538379235031, 1.999999999999998224, -34.00000000000000000 ) ) ;
#4327 = ORIENTED_EDGE ( 'NONE', *, *, #13988, .F. ) ;
#4328 = CARTESIAN_POINT ( 'NONE',  ( -6.473970235329672780E-16, -4.862606272033106691, -3.745885042887442395 ) ) ;
#4329 = ORIENTED_EDGE ( 'NONE', *, *, #11388, .F. ) ;
#4330 = CIRCLE ( 'NONE', #10531, 4.000000000000000000 ) ;
#4331 = VERTEX_POINT ( 'NONE', #7188 ) ;
#4332 = DIRECTION ( 'NONE',  ( 0.000000000000000000, 1.000000000000000000, 0.000000000000000000 ) ) ;
#4333 = CARTESIAN_POINT ( 'NONE',  ( -4.236525694536558362, 2.416953475386465211, -3.751298745799836354 ) ) ;
#4334 = FACE_BOUND ( 'NONE', #8727, .T. ) ;
#4335 = CIRCLE ( 'NONE', #10006, 2.649999999999985700 ) ;
#4336 = ADVANCED_FACE ( 'NONE', ( #6125 ), #703, .F. ) ;
#4337 = CIRCLE ( 'NONE', #7184, 4.000000000000000000 ) ;
#4338 = PRODUCT_RELATED_PRODUCT_CATEGORY ( 'part', '', ( #15460 ) ) ;
#4339 = CARTESIAN_POINT ( 'NONE',  ( 2.071067811865491048, -26.31250000273118417, 4.999999999999985789 ) ) ;
#4340 = CYLINDRICAL_SURFACE ( 'NONE', #7830, 1.999999999999998224 ) ;
#4341 = DIRECTION ( 'NONE',  ( -6.938893903907228378E-16, -1.000000000000000000, 0.000000000000000000 ) ) ;
#4342 = CARTESIAN_POINT ( 'NONE',  ( 35.00000000000000000, 50.00000000000000000, -2.649999999999992806 ) ) ;
#4343 = CARTESIAN_POINT ( 'NONE',  ( 3.061616997868383141E-16, -27.75000000000000000, -5.000000000000000000 ) ) ;
#4344 = CYLINDRICAL_SURFACE ( 'NONE', #14407, 10.00000000000000000 ) ;
#4345 = CARTESIAN_POINT ( 'NONE',  ( 1.846868145590736310, -28.87500000136559564, 4.458734124999997661 ) ) ;
#4346 = CARTESIAN_POINT ( 'NONE',  ( -2.131511515620587272, -3.916244202832140253, 1.312500001365592750 ) ) ;
#4347 = VERTEX_POINT ( 'NONE', #4829 ) ;
#4348 = CARTESIAN_POINT ( 'NONE',  ( 0.6250000000000025535, 8.299410119600878488, -7.298562697733109061 ) ) ;
#4349 = ORIENTED_EDGE ( 'NONE', *, *, #10158, .F. ) ;
#4350 = EDGE_LOOP ( 'NONE', ( #9606, #7636, #8059, #6743, #9250, #12755, #6033, #5360 ) ) ;
#4351 = CONICAL_SURFACE ( 'NONE', #10809, 2.059999999999998721, 0.9599310885968738161 ) ;
#4352 = CARTESIAN_POINT ( 'NONE',  ( -1.846868145590734756, -25.37500000136559919, -4.458734125000000326 ) ) ;
#4353 = CARTESIAN_POINT ( 'NONE',  ( -5.384454397937118664, 6.594054843588581554E-16, -4.484454397937119197 ) ) ;
#4354 = EDGE_LOOP ( 'NONE', ( #2016, #3937, #6611, #9493, #248, #8433 ) ) ;
#4355 = AXIS2_PLACEMENT_3D ( 'NONE', #4226, #9168, #3016 ) ;
#4356 = CARTESIAN_POINT ( 'NONE',  ( 0.000000000000000000, -20.00000000000000000, 0.000000000000000000 ) ) ;
#4357 = EDGE_CURVE ( 'NONE', #11193, #11117, #6040, .T. ) ;
#4358 = PRODUCT_RELATED_PRODUCT_CATEGORY ( 'part', '', ( #9629 ) ) ;
#4359 = ADVANCED_FACE ( 'NONE', ( #3446 ), #8400, .T. ) ;
#4360 = ADVANCED_FACE ( 'NONE', ( #1029, #12326 ), #5964, .F. ) ;
#4361 = CARTESIAN_POINT ( 'NONE',  ( 7.897825807688668043, 1.532833846124465271, -7.633607627188378153 ) ) ;
#4362 = CARTESIAN_POINT ( 'NONE',  ( 2.131511515620586383, 3.916244202832140253, -6.187499998634407028 ) ) ;
#4363 = CYLINDRICAL_SURFACE ( 'NONE', #7560, 2.649999999999985700 ) ;
#4364 = AXIS2_PLACEMENT_3D ( 'NONE', #13597, #2528, #6266 ) ;
#4365 = CARTESIAN_POINT ( 'NONE',  ( 5.000000000000000000, -26.06250000000000355, 2.071067811865478614 ) ) ;
#4366 = CARTESIAN_POINT ( 'NONE',  ( 3.753672977998667726, 3.033343224707664376, -7.249999998634409692 ) ) ;
#4367 = DIRECTION ( 'NONE',  ( -0.000000000000000000, -1.000000000000000000, -0.000000000000000000 ) ) ;
#4368 = DIRECTION ( 'NONE',  ( -0.000000000000000000, -1.000000000000000000, -0.000000000000000000 ) ) ;
#4369 = CARTESIAN_POINT ( 'NONE',  ( 2.071067811865475505, -24.93750000273118772, -5.000000000000000888 ) ) ;
#4370 = ORIENTED_EDGE ( 'NONE', *, *, #4253, .T. ) ;
#4371 = VECTOR ( 'NONE', #11419, 1000.000000000000000 ) ;
#4372 = CARTESIAN_POINT ( 'NONE',  ( -4.458734124999999437, -27.93750000136559564, -5.460374474430324690E-16 ) ) ;
#4373 = CARTESIAN_POINT ( 'NONE',  ( 4.406466114818385904, -6.116179640278937235, -7.446478553995120819 ) ) ;
#4374 = ORIENTED_EDGE ( 'NONE', *, *, #7133, .T. ) ;
#4375 = ORIENTED_EDGE ( 'NONE', *, *, #9521, .T. ) ;
#4376 = CARTESIAN_POINT ( 'NONE',  ( -1.415196051561583790, 4.795541693661363958, -3.624999997268816276 ) ) ;
#4377 = CARTESIAN_POINT ( 'NONE',  ( -60.00000000000000000, -5.000000000000004441, -18.00000000000001066 ) ) ;
#4378 = AXIS2_PLACEMENT_3D ( 'NONE', #3538, #8494, #2329 ) ;
#4379 = ORIENTED_EDGE ( 'NONE', *, *, #8182, .T. ) ;
#4380 = PLANE ( 'NONE',  #3978 ) ;
#4381 = EDGE_CURVE ( 'NONE', #9125, #14724, #2317, .T. ) ;
#4382 = CARTESIAN_POINT ( 'NONE',  ( 39.57820647634153488, -4.462727778340672025, -28.44065064052909975 ) ) ;
#4383 = CARTESIAN_POINT ( 'NONE',  ( 4.458734124999999437, -25.75000000136559564, 1.846868145590737864 ) ) ;
#4384 = DIRECTION ( 'NONE',  ( 0.000000000000000000, 0.000000000000000000, 1.000000000000000000 ) ) ;
#4385 = FACE_OUTER_BOUND ( 'NONE', #14907, .T. ) ;
#4386 = CONTEXT_DEPENDENT_SHAPE_REPRESENTATION ( #5674, #1119 ) ;
#4387 = CARTESIAN_POINT ( 'NONE',  ( 2.071067811865473285, -31.81249999999999289, -5.000000000000002665 ) ) ;
#4388 = VECTOR ( 'NONE', #1311, 1000.000000000000114 ) ;
#4389 = CARTESIAN_POINT ( 'NONE',  ( -3.916244202832140253, 2.131511515620587272, -0.1874999986344084990 ) ) ;
#4390 = EDGE_LOOP ( 'NONE', ( #12843, #346, #15608, #8435 ) ) ;
#4391 = PRESENTATION_STYLE_ASSIGNMENT (( #14248 ) ) ;
#4392 = EDGE_LOOP ( 'NONE', ( #10584, #1758 ) ) ;
#4393 = FACE_OUTER_BOUND ( 'NONE', #5894, .T. ) ;
#4394 = ORIENTED_EDGE ( 'NONE', *, *, #13923, .T. ) ;
#4395 = CONTEXT_DEPENDENT_SHAPE_REPRESENTATION ( #13491, #2607 ) ;
#4396 = DIRECTION ( 'NONE',  ( -1.000000000000000000, 0.000000000000000000, 0.000000000000000000 ) ) ;
#4397 = DIRECTION ( 'NONE',  ( 0.000000000000000000, 0.000000000000000000, 1.000000000000000000 ) ) ;
#4398 = B_SPLINE_CURVE_WITH_KNOTS ( 'NONE', 3,
 ( #6948, #9363, #13144, #5485, #8082, #6861, #10413, #12978 ),
 .UNSPECIFIED., .F., .F.,
 ( 4, 2, 2, 4 ),
 ( 2.465131517071610173E-07, 0.001183067374689837636, 0.001774477805458902699, 0.002365888236227967761 ),
 .UNSPECIFIED. ) ;
#4399 = CARTESIAN_POINT ( 'NONE',  ( 3.916244202832140253, -2.131511515620588160, 1.312500001365592750 ) ) ;
#4400 = CARTESIAN_POINT ( 'NONE',  ( 30.02221399786053624, -35.00000000000000000, -15.99999999999997868 ) ) ;
#4401 = SURFACE_STYLE_FILL_AREA ( #2855 ) ;
#4402 = ORIENTED_EDGE ( 'NONE', *, *, #8108, .F. ) ;
#4403 = CARTESIAN_POINT ( 'NONE',  ( 7.500000000000000888, 1.489914625144004523, -0.1187923833806749097 ) ) ;
#4404 = CARTESIAN_POINT ( 'NONE',  ( -3.401574460001765221, 4.209348295687701302, -2.562499997268814944 ) ) ;
#4405 = DIRECTION ( 'NONE',  ( -1.000000000000000000, -1.541976423090495140E-16, -0.000000000000000000 ) ) ;
#4406 = ADVANCED_FACE ( 'NONE', ( #14764 ), #9831, .T. ) ;
#4407 = ORIENTED_EDGE ( 'NONE', *, *, #8541, .F. ) ;
#4408 = DIRECTION ( 'NONE',  ( 0.000000000000000000, 0.8660254037844380415, -0.5000000000000012212 ) ) ;
#4409 = ORIENTED_EDGE ( 'NONE', *, *, #13196, .T. ) ;
#4410 = ORIENTED_EDGE ( 'NONE', *, *, #9663, .F. ) ;
#4411 = CARTESIAN_POINT ( 'NONE',  ( -9.184850993605147944E-16, -23.37500000273118772, 5.000000000000000000 ) ) ;
#4412 = DIRECTION ( 'NONE',  ( 0.000000000000000000, 1.000000000000000000, 0.000000000000000000 ) ) ;
#4413 = FACE_OUTER_BOUND ( 'NONE', #847, .T. ) ;
#4414 = CARTESIAN_POINT ( 'NONE',  ( -4.795541693661363958, -1.415196051561583790, -5.500000000000001776 ) ) ;
#4415 = FACE_OUTER_BOUND ( 'NONE', #6444, .T. ) ;
#4416 = CARTESIAN_POINT ( 'NONE',  ( 2.071067811865447528, -22.81250000000000000, -5.000000000000029310 ) ) ;
#4417 = CARTESIAN_POINT ( 'NONE',  ( -4.391654775818395251, 2.390265326283148806, -7.625000000000003553 ) ) ;
#4418 = DIRECTION ( 'NONE',  ( -0.000000000000000000, 1.000000000000000000, -0.000000000000000000 ) ) ;
#4419 = CARTESIAN_POINT ( 'NONE',  ( -19.99999999999956657, -9.000000000000001776, -2.499999999999120259 ) ) ;
#4420 = CARTESIAN_POINT ( 'NONE',  ( -4.458734124999999437, -29.25000000136559564, -1.846868145590735644 ) ) ;
#4421 = CARTESIAN_POINT ( 'NONE',  ( 3.753672977998667726, 3.033343224707664376, -1.249999998634407916 ) ) ;
#4422 = VERTEX_POINT ( 'NONE', #7420 ) ;
#4423 = CYLINDRICAL_SURFACE ( 'NONE', #1183, 30.00000000000000711 ) ;
#4424 = EDGE_CURVE ( 'NONE', #13829, #1597, #5343, .T. ) ;
#4425 = ORIENTED_EDGE ( 'NONE', *, *, #12842, .F. ) ;
#4426 = ORIENTED_EDGE ( 'NONE', *, *, #800, .T. ) ;
#4427 = EDGE_CURVE ( 'NONE', #2056, #4537, #1264, .T. ) ;
#4428 =( NAMED_UNIT ( * ) PLANE_ANGLE_UNIT ( ) SI_UNIT ( $, .RADIAN. ) );
#4429 = CARTESIAN_POINT ( 'NONE',  ( 4.458734125000000326, -27.62500000136559564, -1.846868145590734978 ) ) ;
#4430 = DIRECTION ( 'NONE',  ( 1.000000000000000000, 1.239088197126290324E-16, -0.000000000000000000 ) ) ;
#4431 = CARTESIAN_POINT ( 'NONE',  ( 4.999999999999845457, -1.272547481429021854, -6.086597482644649837 ) ) ;
#4432 = LINE ( 'NONE', #5649, #3574 ) ;
#4433 = CARTESIAN_POINT ( 'NONE',  ( -0.5093500532425060401, -4.799145180956616130, -4.624999998634405252 ) ) ;
#4434 = CARTESIAN_POINT ( 'NONE',  ( 1.567478505476134606E-15, 4.618802153517012066, -3.433295621305382905 ) ) ;
#4435 = CARTESIAN_POINT ( 'NONE',  ( -5.000000000000000000, -25.50000000000000355, -6.123233995736766282E-16 ) ) ;
#4436 = CARTESIAN_POINT ( 'NONE',  ( -4.795541693661363958, -1.415196051561583790, 1.499999999999997780 ) ) ;
#4437 = DIRECTION ( 'NONE',  ( 0.000000000000000000, 0.000000000000000000, -1.000000000000000000 ) ) ;
#4438 = DIRECTION ( 'NONE',  ( -1.000000000000000000, 0.000000000000000000, 0.000000000000000000 ) ) ;
#4439 = CARTESIAN_POINT ( 'NONE',  ( 3.152801135295366208, -29.56250000136559208, 3.152801135295367985 ) ) ;
#4440 = VERTEX_POINT ( 'NONE', #2386 ) ;
#4441 = CARTESIAN_POINT ( 'NONE',  ( 4.458734124999999437, -21.43750000136559208, 0.000000000000000000 ) ) ;
#4442 = APPLICATION_CONTEXT ( 'automotive_design' ) ;
#4443 = ADVANCED_FACE ( 'NONE', ( #2874 ), #11200, .F. ) ;
#4444 = FACE_BOUND ( 'NONE', #945, .T. ) ;
#4445 = ORIENTED_EDGE ( 'NONE', *, *, #15324, .T. ) ;
#4446 = EDGE_LOOP ( 'NONE', ( #12730, #3586 ) ) ;
#4447 = EDGE_CURVE ( 'NONE', #5406, #13669, #1583, .T. ) ;
#4448 = CARTESIAN_POINT ( 'NONE',  ( 7.499999999999999112, -2.930060224340428121, -0.4701183149080244705 ) ) ;
#4449 = DIRECTION ( 'NONE',  ( 1.000000000000000000, 0.000000000000000000, 0.000000000000000000 ) ) ;
#4450 = ORIENTED_EDGE ( 'NONE', *, *, #7947, .T. ) ;
#4451 = CARTESIAN_POINT ( 'NONE',  ( 5.000000000000004441, -2.247904837838113790E-16, -2.045263047592944528 ) ) ;
#4452 = DIRECTION ( 'NONE',  ( -1.000000000000000000, 0.000000000000000000, -0.000000000000000000 ) ) ;
#4453 = CARTESIAN_POINT ( 'NONE',  ( -1.846868145590734756, -28.37500000136559564, -4.458734125000000326 ) ) ;
#4454 = DIRECTION ( 'NONE',  ( -0.000000000000000000, -1.000000000000000000, -0.000000000000000000 ) ) ;
#4455 = DIRECTION ( 'NONE',  ( -0.000000000000000000, -1.000000000000000000, -0.000000000000000000 ) ) ;
#4456 = DIRECTION ( 'NONE',  ( 0.000000000000000000, 0.000000000000000000, 1.000000000000000000 ) ) ;
#4457 = CIRCLE ( 'NONE', #11675, 2.499999999999998668 ) ;
#4458 = DIRECTION ( 'NONE',  ( 0.000000000000000000, 0.000000000000000000, 1.000000000000000000 ) ) ;
#4459 = LINE ( 'NONE', #12933, #3001 ) ;
#4460 = EDGE_LOOP ( 'NONE', ( #4182, #1228, #1093, #1757, #5956, #11970, #2888, #10877, #11819 ) ) ;
#4461 = EDGE_CURVE ( 'NONE', #8490, #12673, #12283, .T. ) ;
#4462 =( LENGTH_UNIT ( ) NAMED_UNIT ( * ) SI_UNIT ( .MILLI., .METRE. ) );
#4463 = ORIENTED_EDGE ( 'NONE', *, *, #8142, .F. ) ;
#4464 = CARTESIAN_POINT ( 'NONE',  ( -4.419133455864435511, 6.108866147516203604, -7.026396753507444082 ) ) ;
#4465 = B_SPLINE_CURVE_WITH_KNOTS ( 'NONE', 3,
 ( #6614, #9049, #13952, #10339, #15265, #9124 ),
 .UNSPECIFIED., .F., .F.,
 ( 4, 2, 4 ),
 ( 0.000000000000000000, 0.0004189869898914129693, 0.0008379739797828259385 ),
 .UNSPECIFIED. ) ;
#4466 = ORIENTED_EDGE ( 'NONE', *, *, #7538, .F. ) ;
#4467 = AXIS2_PLACEMENT_3D ( 'NONE', #11083, #8823, #14055 ) ;
#4468 = CARTESIAN_POINT ( 'NONE',  ( 16.49999999999956657, -8.786575603324269439E-13, 1.500000000000000000 ) ) ;
#4469 = VECTOR ( 'NONE', #7281, 1000.000000000000000 ) ;
#4470 = CARTESIAN_POINT ( 'NONE',  ( 44.82050807568875683, 0.000000000000000000, 37.63139720814412925 ) ) ;
#4471 = DIRECTION ( 'NONE',  ( 1.000000000000000000, 0.000000000000000000, 0.000000000000000000 ) ) ;
#4472 = CARTESIAN_POINT ( 'NONE',  ( -5.381735091635034607, 0.5711823568785950878, -6.437499997268815832 ) ) ;
#4473 = DIRECTION ( 'NONE',  ( -0.8660254037844387076, 0.000000000000000000, 0.4999999999999997224 ) ) ;
#4474 = CARTESIAN_POINT ( 'NONE',  ( -4.197393957002303999, -0.8151795401431414234, -3.503767560748935139 ) ) ;
#4475 = FACE_OUTER_BOUND ( 'NONE', #13518, .T. ) ;
#4476 = ORIENTED_EDGE ( 'NONE', *, *, #6647, .F. ) ;
#4477 = CARTESIAN_POINT ( 'NONE',  ( 0.000000000000000000, 0.000000000000000000, 0.000000000000000000 ) ) ;
#4478 = CARTESIAN_POINT ( 'NONE',  ( 2.467663300281918126E-15, 50.00000000000000000, -70.14999999999999147 ) ) ;
#4479 = EDGE_CURVE ( 'NONE', #9721, #7795, #15171, .T. ) ;
#4480 = DIRECTION ( 'NONE',  ( -0.000000000000000000, -0.000000000000000000, 1.000000000000000000 ) ) ;
#4481 = ORIENTED_EDGE ( 'NONE', *, *, #11590, .F. ) ;
#4482 = FACE_OUTER_BOUND ( 'NONE', #14641, .T. ) ;
#4483 = ORIENTED_EDGE ( 'NONE', *, *, #8975, .F. ) ;
#4484 = ORIENTED_EDGE ( 'NONE', *, *, #6938, .T. ) ;
#4485 = CARTESIAN_POINT ( 'NONE',  ( -5.000000000000000888, -30.56250000000000000, -2.071067811865475949 ) ) ;
#4486 = DIRECTION ( 'NONE',  ( 0.000000000000000000, 0.000000000000000000, 1.000000000000000000 ) ) ;
#4487 = CYLINDRICAL_SURFACE ( 'NONE', #12754, 10.00000000000000000 ) ;
#4488 = EDGE_CURVE ( 'NONE', #6791, #7896, #9226, .T. ) ;
#4489 = CARTESIAN_POINT ( 'NONE',  ( -0.5711823568785977523, -5.381735091635034607, -5.312499999999999112 ) ) ;
#4490 = PLANE ( 'NONE',  #3423 ) ;
#4491 = CARTESIAN_POINT ( 'NONE',  ( 4.000000000000000000, -1.560351142792952617, -0.2242961665059816367 ) ) ;
#4492 =( GEOMETRIC_REPRESENTATION_CONTEXT ( 3 ) GLOBAL_UNCERTAINTY_ASSIGNED_CONTEXT ( ( #2527 ) ) GLOBAL_UNIT_ASSIGNED_CONTEXT ( ( #14882, #14554, #1132 ) ) REPRESENTATION_CONTEXT ( 'NONE', 'WORKASPACE' ) );
#4493 = DIRECTION ( 'NONE',  ( 0.000000000000000000, 0.000000000000000000, -1.000000000000000000 ) ) ;
#4494 = CARTESIAN_POINT ( 'NONE',  ( 0.000000000000000000, 0.000000000000000000, 0.000000000000000000 ) ) ;
#4495 = DIRECTION ( 'NONE',  ( 0.000000000000000000, 0.000000000000000000, 1.000000000000000000 ) ) ;
#4496 = CARTESIAN_POINT ( 'NONE',  ( -3.152801135295367985, -31.06250000136559564, 3.152801135295367096 ) ) ;
#4497 = CARTESIAN_POINT ( 'NONE',  ( -1.261996585732579224, 4.276409079477648589, -2.062499998634406584 ) ) ;
#4498 = EDGE_LOOP ( 'NONE', ( #14987, #11958 ) ) ;
#4499 = CARTESIAN_POINT ( 'NONE',  ( 6.484173630540333910, 4.916614646778451281, -7.642786413620781261 ) ) ;
#4500 = VERTEX_POINT ( 'NONE', #2630 ) ;
#4501 = ORIENTED_EDGE ( 'NONE', *, *, #3581, .T. ) ;
#4502 = CARTESIAN_POINT ( 'NONE',  ( 3.152801135295366208, -26.81250000136559564, 3.152801135295367985 ) ) ;
#4503 = CARTESIAN_POINT ( 'NONE',  ( 4.209348295687701302, 3.401574460001766109, -7.937500000000003553 ) ) ;
#4504 = AXIS2_PLACEMENT_3D ( 'NONE', #14728, #14563, #8206 ) ;
#4505 = AXIS2_PLACEMENT_3D ( 'NONE', #4825, #9829, #4905 ) ;
#4506 = CARTESIAN_POINT ( 'NONE',  ( -5.000000000000000888, -29.43750000000000711, 2.071067811865474617 ) ) ;
#4507 = EDGE_CURVE ( 'NONE', #12690, #3419, #5064, .T. ) ;
#4508 = CARTESIAN_POINT ( 'NONE',  ( -3.033343224707664820, 3.753672977998667726, -6.999999998634409692 ) ) ;
#4509 = DIRECTION ( 'NONE',  ( 0.000000000000000000, 0.000000000000000000, -1.000000000000000000 ) ) ;
#4510 = EDGE_CURVE ( 'NONE', #11190, #11803, #13982, .T. ) ;
#4511 = CARTESIAN_POINT ( 'NONE',  ( 5.000000000000000000, -27.06250000000000000, 2.071067811865478614 ) ) ;
#4512 = CARTESIAN_POINT ( 'NONE',  ( -3.916244202832140253, 2.131511515620587272, -6.937499998634407916 ) ) ;
#4513 = CARTESIAN_POINT ( 'NONE',  ( 67.49999999999931788, 37.00000000000000000, 2.081668171172168513E-14 ) ) ;
#4514 = DIRECTION ( 'NONE',  ( 1.000000000000000000, 0.000000000000000000, 0.000000000000000000 ) ) ;
#4515 = CARTESIAN_POINT ( 'NONE',  ( -3.152801135295367985, -30.81250000136559564, 3.152801135295367096 ) ) ;
#4516 = ORIENTED_EDGE ( 'NONE', *, *, #4313, .F. ) ;
#4517 = PRESENTATION_LAYER_ASSIGNMENT (  '', '', ( #398 ) ) ;
#4518 = CARTESIAN_POINT ( 'NONE',  ( 1.846868145590736310, -23.62500000136559564, 4.458734124999997661 ) ) ;
#4519 = FACE_BOUND ( 'NONE', #8353, .T. ) ;
#4520 = ORIENTED_EDGE ( 'NONE', *, *, #7044, .F. ) ;
#4521 = ORIENTED_EDGE ( 'NONE', *, *, #5203, .F. ) ;
#4523 = CARTESIAN_POINT ( 'NONE',  ( 4.000000000000000000, -2.309401076758514915, -3.433295621305383349 ) ) ;
#4522 = VECTOR ( 'NONE', #5281, 1000.000000000000000 ) ;
#4524 = CARTESIAN_POINT ( 'NONE',  ( 4.458734124999999437, -28.50000000136559564, 1.846868145590737864 ) ) ;
#4525 = CARTESIAN_POINT ( 'NONE',  ( -4.795541693661363958, -1.415196051561583790, -7.374999997268815832 ) ) ;
#4526 = EDGE_LOOP ( 'NONE', ( #14542, #13389, #13917, #11725 ) ) ;
#4527 = DIRECTION ( 'NONE',  ( 0.000000000000000000, 0.000000000000000000, -1.000000000000000000 ) ) ;
#4528 = AXIS2_PLACEMENT_3D ( 'NONE', #15021, #156, #9842 ) ;
#4529 = DIRECTION ( 'NONE',  ( -1.000000000000000000, 0.000000000000000000, 0.000000000000000000 ) ) ;
#4530 = ADVANCED_FACE ( 'NONE', ( #1660 ), #14889, .T. ) ;
#4531 = VECTOR ( 'NONE', #13656, 1000.000000000000114 ) ;
#4532 = CARTESIAN_POINT ( 'NONE',  ( -3.152801135295367096, -28.31250000136559564, -3.152801135295367541 ) ) ;
#4533 = DIRECTION ( 'NONE',  ( 0.000000000000000000, 0.000000000000000000, -1.000000000000000000 ) ) ;
#4534 = DIRECTION ( 'NONE',  ( -0.000000000000000000, 1.000000000000000000, -0.000000000000000000 ) ) ;
#4535 = CARTESIAN_POINT ( 'NONE',  ( -36.99999999999999289, -11.00000000000000178, -3.999999999999170885 ) ) ;
#4536 = CARTESIAN_POINT ( 'NONE',  ( 4.207491450040567571, -2.029819825146485179, -3.671670828759567407 ) ) ;
#4537 = VERTEX_POINT ( 'NONE', #4089 ) ;
#4538 = VECTOR ( 'NONE', #14752, 1000.000000000000000 ) ;
#4539 =( LENGTH_UNIT ( ) NAMED_UNIT ( * ) SI_UNIT ( .MILLI., .METRE. ) );
#4540 = VERTEX_POINT ( 'NONE', #12403 ) ;
#4541 = CARTESIAN_POINT ( 'NONE',  ( 0.000000000000000000, 0.000000000000000000, -9.226681596905677907 ) ) ;
#4542 = VERTEX_POINT ( 'NONE', #12721 ) ;
#4543 = CARTESIAN_POINT ( 'NONE',  ( -5.000000000000000888, -26.56250000000000000, -2.071067811865475949 ) ) ;
#4544 = ADVANCED_FACE ( 'NONE', ( #6603 ), #13616, .F. ) ;
#4545 = ADVANCED_FACE ( 'NONE', ( #11286 ), #9040, .F. ) ;
#4546 = EDGE_CURVE ( 'NONE', #5482, #13690, #7503, .T. ) ;
#4547 = VECTOR ( 'NONE', #6917, 1000.000000000000000 ) ;
#4548 = CARTESIAN_POINT ( 'NONE',  ( 0.3198814748697593746, 4.434118497892183264, -0.3507732604232499107 ) ) ;
#4549 = CARTESIAN_POINT ( 'NONE',  ( 4.276409079477644148, 1.261996585732577891, 0.6875000013655923059 ) ) ;
#4550 = CARTESIAN_POINT ( 'NONE',  ( 0.000000000000000000, -30.00000000000000355, 0.000000000000000000 ) ) ;
#4551 = AXIS2_PLACEMENT_3D ( 'NONE', #6245, #14974, #11158 ) ;
#4552 = CARTESIAN_POINT ( 'NONE',  ( 0.5093500532425063732, 4.799145180956616130, -3.374999998634407472 ) ) ;
#4553 = CARTESIAN_POINT ( 'NONE',  ( -1.415196051561583790, 4.795541693661363958, -0.7500000000000006661 ) ) ;
#4554 = CARTESIAN_POINT ( 'NONE',  ( 7.922281120364393914, -4.573931137438281169, -8.047472243342932430 ) ) ;
#4555 = ORIENTED_EDGE ( 'NONE', *, *, #8556, .F. ) ;
#4556 = CARTESIAN_POINT ( 'NONE',  ( 14.41154273188008439, 88.59290746114278647, 60.96152422706632024 ) ) ;
#4557 = DIRECTION ( 'NONE',  ( -0.5000000000000004441, 0.8660254037844383745, 0.000000000000000000 ) ) ;
#4558 = LINE ( 'NONE', #8370, #4547 ) ;
#4559 = ORIENTED_EDGE ( 'NONE', *, *, #13542, .T. ) ;
#4560 = FACE_OUTER_BOUND ( 'NONE', #10471, .T. ) ;
#4561 = VECTOR ( 'NONE', #236, 1000.000000000000114 ) ;
#4562 = ORIENTED_EDGE ( 'NONE', *, *, #4357, .F. ) ;
#4563 = VERTEX_POINT ( 'NONE', #1421 ) ;
#4564 = CARTESIAN_POINT ( 'NONE',  ( 1.261996585732578113, -4.276409079477644148, -0.8124999986344090264 ) ) ;
#4565 = DIRECTION ( 'NONE',  ( -0.000000000000000000, -0.000000000000000000, 1.000000000000000000 ) ) ;
#4566 = PRESENTATION_STYLE_ASSIGNMENT (( #2131 ) ) ;
#4567 = EDGE_CURVE ( 'NONE', #7493, #3963, #6451, .T. ) ;
#4568 = PLANE ( 'NONE',  #4320 ) ;
#4570 = LINE ( 'NONE', #9505, #7053 ) ;
#4569 = VECTOR ( 'NONE', #14181, 1000.000000000000000 ) ;
#4571 = CARTESIAN_POINT ( 'NONE',  ( 3.999999999999999112, -0.7890432684750902093, -0.04868663549882291247 ) ) ;
#4572 = CARTESIAN_POINT ( 'NONE',  ( 2.390265326283148806, 4.391654775818395251, -7.875000000000003553 ) ) ;
#4573 = DIRECTION ( 'NONE',  ( 0.000000000000000000, -1.000000000000000000, 1.287488025362403787E-15 ) ) ;
#4574 = CARTESIAN_POINT ( 'NONE',  ( -8.190561711645485556E-16, -28.93750000136559564, 4.458734124999999437 ) ) ;
#4575 = CARTESIAN_POINT ( 'NONE',  ( 4.276409079477644148, 1.261996585732577891, 0.6875000013655923059 ) ) ;
#4576 = ORIENTED_EDGE ( 'NONE', *, *, #475, .F. ) ;
#4577 = CARTESIAN_POINT ( 'NONE',  ( 2.387978478800976134, 7.281554020289609852, -7.069802615102036114 ) ) ;
#4578 = ORIENTED_EDGE ( 'NONE', *, *, #7311, .T. ) ;
#4579 = ORIENTED_EDGE ( 'NONE', *, *, #12723, .T. ) ;
#4580 = ORIENTED_EDGE ( 'NONE', *, *, #14027, .T. ) ;
#4581 = CARTESIAN_POINT ( 'NONE',  ( -1.846868145590734756, -28.37500000136559564, -4.458734125000000326 ) ) ;
#4582 = AXIS2_PLACEMENT_3D ( 'NONE', #13894, #8982, #7777 ) ;
#4583 = DIRECTION ( 'NONE',  ( -0.8660254037844388186, 0.000000000000000000, 0.4999999999999997780 ) ) ;
#4584 = AXIS2_PLACEMENT_3D ( 'NONE', #3360, #8617, #13274 ) ;
#4585 = CARTESIAN_POINT ( 'NONE',  ( 2.500000000000000000, 1.768423874527822681, -1.021000000000002794 ) ) ;
#4586 = AXIS2_PLACEMENT_3D ( 'NONE', #6316, #11232, #1213 ) ;
#4587 = CARTESIAN_POINT ( 'NONE',  ( 4.799145180956616130, -0.5093500532425063732, -7.374999998634407916 ) ) ;
#4588 = CARTESIAN_POINT ( 'NONE',  ( -15.99999999999979217, -11.00000000000000178, 1.499999999999998890 ) ) ;
#4589 = PLANE ( 'NONE',  #1527 ) ;
#4590 = CARTESIAN_POINT ( 'NONE',  ( -2.131511515620587272, -3.916244202832140253, -7.687499998634407916 ) ) ;
#4591 = CARTESIAN_POINT ( 'NONE',  ( -60.00000000000000000, -37.00000000000000711, -20.00000000000000711 ) ) ;
#4592 = CARTESIAN_POINT ( 'NONE',  ( 39.53738644056385709, 0.000000000000000000, 28.48076211354143794 ) ) ;
#4593 = CARTESIAN_POINT ( 'NONE',  ( -3.152801135295367985, -28.81250000136559564, 3.152801135295367096 ) ) ;
#4594 = VERTEX_POINT ( 'NONE', #10160 ) ;
#4595 = LINE ( 'NONE', #14384, #1221 ) ;
#4596 = CARTESIAN_POINT ( 'NONE',  ( 17.00000000000000000, 2.055000000000000160, 0.000000000000000000 ) ) ;
#4597 = VERTEX_POINT ( 'NONE', #12961 ) ;
#4598 = VERTEX_POINT ( 'NONE', #1744 ) ;
#4599 = CARTESIAN_POINT ( 'NONE',  ( -90.00000000000000000, -95.00000000000000000, -7.500000000000000000 ) ) ;
#4600 = AXIS2_PLACEMENT_3D ( 'NONE', #616, #11820, #771 ) ;
#4601 = CARTESIAN_POINT ( 'NONE',  ( 3.152801135295366208, -30.56250000136559564, 3.152801135295367985 ) ) ;
#4602 = EDGE_CURVE ( 'NONE', #9091, #13173, #9194, .T. ) ;
#4603 = DIRECTION ( 'NONE',  ( -0.000000000000000000, 1.000000000000000000, -0.000000000000000000 ) ) ;
#4604 =( BOUNDED_CURVE ( )  B_SPLINE_CURVE ( 2, ( #13273, #2302, #13199, #1162, #15809, #2065, #6104, #12147, #2214 ),
 .UNSPECIFIED., .F., .F. ) 
 B_SPLINE_CURVE_WITH_KNOTS ( ( 3, 2, 2, 2, 3 ),
 ( 0.1250000000000001110, 0.1375000000000001221, 0.1500000000000001332, 0.1625000000000001443, 0.1750000000000001554 ),
 .UNSPECIFIED. ) 
 CURVE ( )  GEOMETRIC_REPRESENTATION_ITEM ( )  RATIONAL_B_SPLINE_CURVE ( ( 0.9999999999999993339, 0.9238795325112874046, 1.000000000000000000, 0.9238795325112867385, 1.000000000000000000, 0.9238795325112867385, 1.000000000000000000, 0.9238795325112857393, 1.000000000000001110 ) ) 
 REPRESENTATION_ITEM ( '' )  );
#4605 = ORIENTED_EDGE ( 'NONE', *, *, #15904, .F. ) ;
#4606 = DIRECTION ( 'NONE',  ( 0.000000000000000000, 0.000000000000000000, 1.000000000000000000 ) ) ;
#4607 = VECTOR ( 'NONE', #12069, 1000.000000000000000 ) ;
#4608 =( GEOMETRIC_REPRESENTATION_CONTEXT ( 3 ) GLOBAL_UNCERTAINTY_ASSIGNED_CONTEXT ( ( #14034 ) ) GLOBAL_UNIT_ASSIGNED_CONTEXT ( ( #2199, #15793, #10932 ) ) REPRESENTATION_CONTEXT ( 'NONE', 'WORKASPACE' ) );
#4609 = PRODUCT_DEFINITION_SHAPE ( 'NONE', 'NONE',  #4824 ) ;
#4610 = FACE_OUTER_BOUND ( 'NONE', #8642, .T. ) ;
#4611 = LINE ( 'NONE', #8275, #9365 ) ;
#4612 = PRESENTATION_LAYER_ASSIGNMENT (  '', '', ( #12861 ) ) ;
#4613 = CARTESIAN_POINT ( 'NONE',  ( 1.846868145590736310, -23.87500000136559564, 4.458734124999999437 ) ) ;
#4614 = VECTOR ( 'NONE', #1707, 1000.000000000000000 ) ;
#4615 = CYLINDRICAL_SURFACE ( 'NONE', #6248, 25.00000000000000000 ) ;
#4616 = CYLINDRICAL_SURFACE ( 'NONE', #3572, 2.000000000000001332 ) ;
#4617 = DIRECTION ( 'NONE',  ( -0.000000000000000000, 1.000000000000000000, -0.000000000000000000 ) ) ;
#4618 = DIRECTION ( 'NONE',  ( 0.000000000000000000, 0.000000000000000000, -1.000000000000000000 ) ) ;
#4619 = AXIS2_PLACEMENT_3D ( 'NONE', #5093, #12506, #6633 ) ;
#4620 = VERTEX_POINT ( 'NONE', #14113 ) ;
#4621 = AXIS2_PLACEMENT_3D ( 'NONE', #14233, #2988, #7941 ) ;
#4622 = SURFACE_SIDE_STYLE ('',( #5519 ) ) ;
#4624 = ORIENTED_EDGE ( 'NONE', *, *, #145, .T. ) ;
#4623 = EDGE_CURVE ( 'NONE', #8700, #13974, #9423, .T. ) ;
#4625 = CARTESIAN_POINT ( 'NONE',  ( -5.112021521198794716, 5.708827036477132744, -7.069802615102390497 ) ) ;
#4626 = ADVANCED_FACE ( 'NONE', ( #1981 ), #14353, .T. ) ;
#4627 = VERTEX_POINT ( 'NONE', #702 ) ;
#4628 = CARTESIAN_POINT ( 'NONE',  ( -9.184850993605147944E-16, -26.25000000000000355, 5.000000000000000000 ) ) ;
#4629 = DIRECTION ( 'NONE',  ( -1.000000000000000000, 1.224646799147354686E-16, 0.000000000000000000 ) ) ;
#4630 = ORIENTED_EDGE ( 'NONE', *, *, #8121, .T. ) ;
#4631 = FACE_OUTER_BOUND ( 'NONE', #14557, .T. ) ;
#4632 = DIRECTION ( 'NONE',  ( -1.000000000000000000, 0.000000000000000000, 0.000000000000000000 ) ) ;
#4633 = CARTESIAN_POINT ( 'NONE',  ( -4.799145180956616130, 0.5093500532425063732, -2.124999998634406584 ) ) ;
#4634 = DIRECTION ( 'NONE',  ( 0.000000000000000000, 0.000000000000000000, 1.000000000000000000 ) ) ;
#4635 = CARTESIAN_POINT ( 'NONE',  ( 3.861362476283255685, 2.629030857715988656, -3.671615880910370500 ) ) ;
#4636 = ORIENTED_EDGE ( 'NONE', *, *, #13750, .F. ) ;
#4637 = CARTESIAN_POINT ( 'NONE',  ( -36.99999999999999289, -13.00000000000000178, 4.000000000000832223 ) ) ;
#4638 = DIRECTION ( 'NONE',  ( 1.000000000000000000, 0.000000000000000000, 0.000000000000000000 ) ) ;
#4639 = EDGE_CURVE ( 'NONE', #4331, #13609, #15498, .T. ) ;
#4640 = ORIENTED_EDGE ( 'NONE', *, *, #4912, .F. ) ;
#4641 = CARTESIAN_POINT ( 'NONE',  ( 2.500000000000000000, 0.000000000000000000, 0.000000000000000000 ) ) ;
#4642 = VERTEX_POINT ( 'NONE', #14022 ) ;
#4643 = EDGE_CURVE ( 'NONE', #6800, #6071, #9114, .T. ) ;
#4644 = VECTOR ( 'NONE', #6675, 1000.000000000000000 ) ;
#4645 = EDGE_LOOP ( 'NONE', ( #7116, #4799, #13900, #5382 ) ) ;
#4646 = DIRECTION ( 'NONE',  ( -0.8660254037844388186, 0.000000000000000000, 0.4999999999999997780 ) ) ;
#4647 = CARTESIAN_POINT ( 'NONE',  ( 0.000000000000000000, 40.00000000000000000, 0.000000000000000000 ) ) ;
#4648 = DIRECTION ( 'NONE',  ( 0.000000000000000000, 0.000000000000000000, 1.000000000000000000 ) ) ;
#4649 = CARTESIAN_POINT ( 'NONE',  ( -9.184850993605147944E-16, -25.25000000000000000, 5.000000000000000000 ) ) ;
#4650 = LINE ( 'NONE', #3429, #13624 ) ;
#4651 = CARTESIAN_POINT ( 'NONE',  ( 5.381735091635035495, -0.5711823568785978633, -0.9374999972688153882 ) ) ;
#4652 = CARTESIAN_POINT ( 'NONE',  ( -2.071067811865475061, -24.68750000000000355, -5.000000000000000888 ) ) ;
#4653 = CARTESIAN_POINT ( 'NONE',  ( -3.535533905932738641, -22.50000000273118772, 3.535533905932737309 ) ) ;
#4654 = CARTESIAN_POINT ( 'NONE',  ( 4.458734124999999437, -30.68750000136559564, 0.000000000000000000 ) ) ;
#4655 = CARTESIAN_POINT ( 'NONE',  ( 0.5093500532425063732, 4.799145180956616130, 0.8750000013655920839 ) ) ;
#4656 = ORIENTED_EDGE ( 'NONE', *, *, #7809, .T. ) ;
#4657 = CARTESIAN_POINT ( 'NONE',  ( 42.02221399786069611, -3.000000000000000000, 2.650000000000096723 ) ) ;
#4658 = EDGE_CURVE ( 'NONE', #2247, #14425, #13142, .T. ) ;
#4659 = ORIENTED_EDGE ( 'NONE', *, *, #275, .F. ) ;
#4660 = ORIENTED_EDGE ( 'NONE', *, *, #9790, .T. ) ;
#4661 = ADVANCED_FACE ( 'NONE', ( #13042 ), #550, .F. ) ;
#4662 = PRESENTATION_STYLE_ASSIGNMENT (( #1996 ) ) ;
#4663 = VERTEX_POINT ( 'NONE', #5628 ) ;
#4664 = CARTESIAN_POINT ( 'NONE',  ( -1.846868145590734756, -27.37500000136559564, -4.458734125000000326 ) ) ;
#4665 = FACE_OUTER_BOUND ( 'NONE', #13563, .T. ) ;
#4666 = CARTESIAN_POINT ( 'NONE',  ( 31.75426480542500229, -5.000000000000000000, -14.99999999999233324 ) ) ;
#4667 = DIRECTION ( 'NONE',  ( 0.000000000000000000, 0.000000000000000000, 1.000000000000000000 ) ) ;
#4668 = CARTESIAN_POINT ( 'NONE',  ( 0.000000000000000000, -13.00000000000000178, 1.500000000000000000 ) ) ;
#4669 = CARTESIAN_POINT ( 'NONE',  ( -3.535533905932738641, -23.37500000000000000, 3.535533905932737309 ) ) ;
#4670 = CARTESIAN_POINT ( 'NONE',  ( 0.5711823568785989735, 5.381735091635026613, -0.8124999999999997780 ) ) ;
#4671 = LINE ( 'NONE', #3379, #2942 ) ;
#4672 = CARTESIAN_POINT ( 'NONE',  ( 3.768577604424125038, -3.256865806044285439, -0.01833770324489448003 ) ) ;
#4673 = CARTESIAN_POINT ( 'NONE',  ( 3.152801135295367541, -31.31250000136559564, -3.152801135295367541 ) ) ;
#4674 = ORIENTED_EDGE ( 'NONE', *, *, #6006, .F. ) ;
#4675 = CARTESIAN_POINT ( 'NONE',  ( -81.33974596215556119, -99.99999999999998579, 7.500000000000001776 ) ) ;
#4676 = ORIENTED_EDGE ( 'NONE', *, *, #6671, .F. ) ;
#4677 = ORIENTED_EDGE ( 'NONE', *, *, #3307, .F. ) ;
#4678 = FACE_OUTER_BOUND ( 'NONE', #8219, .T. ) ;
#4679 = EDGE_CURVE ( 'NONE', #5955, #1559, #13318, .T. ) ;
#4680 = CARTESIAN_POINT ( 'NONE',  ( 4.458734124999999437, -28.43750000136559564, 0.000000000000000000 ) ) ;
#4681 = DIRECTION ( 'NONE',  ( 0.000000000000000000, 0.000000000000000000, 1.000000000000000000 ) ) ;
#4682 = ORIENTED_EDGE ( 'NONE', *, *, #8054, .T. ) ;
#4683 = DIRECTION ( 'NONE',  ( 0.8660254037844383745, 0.000000000000000000, 0.5000000000000005551 ) ) ;
#4684 = PLANE ( 'NONE',  #7411 ) ;
#4685 = CARTESIAN_POINT ( 'NONE',  ( -2.688821387764050996E-14, -4.618802153517012954, -0.4999999999999995559 ) ) ;
#4686 = LINE ( 'NONE', #1940, #3420 ) ;
#4687 = CARTESIAN_POINT ( 'NONE',  ( -4.458734125000001214, -23.12500000136559564, 1.846868145590734089 ) ) ;
#4688 = DIRECTION ( 'NONE',  ( 1.000000000000000000, 0.000000000000000000, 0.000000000000000000 ) ) ;
#4689 = EDGE_CURVE ( 'NONE', #2036, #13476, #9931, .T. ) ;
#4690 = LINE ( 'NONE', #13647, #12865 ) ;
#4691 = FACE_OUTER_BOUND ( 'NONE', #13953, .T. ) ;
#4692 = LINE ( 'NONE', #14552, #8468 ) ;
#4693 = VECTOR ( 'NONE', #15698, 1000.000000000000000 ) ;
#4694 = ORIENTED_EDGE ( 'NONE', *, *, #4947, .T. ) ;
#4695 =( BOUNDED_CURVE ( )  B_SPLINE_CURVE ( 2, ( #8150, #14358, #11604, #8072, #4173, #555, #12893, #7907, #787 ),
 .UNSPECIFIED., .F., .F. ) 
 B_SPLINE_CURVE_WITH_KNOTS ( ( 3, 2, 2, 2, 3 ),
 ( 0.5750000000000001776, 0.5875000000000002442, 0.6000000000000001998, 0.6125000000000002665, 0.6250000000000002220 ),
 .UNSPECIFIED. ) 
 CURVE ( )  GEOMETRIC_REPRESENTATION_ITEM ( )  RATIONAL_B_SPLINE_CURVE ( ( 0.9999999999999986677, 0.9238795325112880708, 1.000000000000000000, 0.9238795325112867385, 1.000000000000000000, 0.9238795325112867385, 1.000000000000000000, 0.9238795325112854062, 1.000000000000001332 ) ) 
 REPRESENTATION_ITEM ( '' )  );
#4696 = SHAPE_REPRESENTATION ( 'hex flange nut gradea_iso_ISO - 4161 - M5 - N', ( #3223 ), #5546 ) ;
#4697 =( NAMED_UNIT ( * ) SI_UNIT ( $, .STERADIAN. ) SOLID_ANGLE_UNIT ( ) );
#4698 = VERTEX_POINT ( 'NONE', #1898 ) ;
#4699 = CARTESIAN_POINT ( 'NONE',  ( 2.682243648011666703, 3.070208061305304881, -0.04852650426601266831 ) ) ;
#4700 = ORIENTED_EDGE ( 'NONE', *, *, #12142, .F. ) ;
#4701 = CARTESIAN_POINT ( 'NONE',  ( 2.500000000000000000, 1.178949249685213863, -2.042000000000001148 ) ) ;
#4702 =( GEOMETRIC_REPRESENTATION_CONTEXT ( 3 ) GLOBAL_UNCERTAINTY_ASSIGNED_CONTEXT ( ( #11448 ) ) GLOBAL_UNIT_ASSIGNED_CONTEXT ( ( #14334, #1068, #920 ) ) REPRESENTATION_CONTEXT ( 'NONE', 'WORKASPACE' ) );
#4703 = CARTESIAN_POINT ( 'NONE',  ( 0.000000000000000000, 2.357898499370433054, -1.951563910473907981E-15 ) ) ;
#4704 = ADVANCED_FACE ( 'NONE', ( #7007 ), #9276, .T. ) ;
#4705 = VECTOR ( 'NONE', #8714, 1000.000000000000000 ) ;
#4706 = CARTESIAN_POINT ( 'NONE',  ( 3.033343224707661712, -3.753672977998669946, -1.499999998634408138 ) ) ;
#4707 = EDGE_CURVE ( 'NONE', #9986, #13690, #8202, .T. ) ;
#4708 = DIRECTION ( 'NONE',  ( 6.123233995736766036E-17, 1.000000000000000000, 0.000000000000000000 ) ) ;
#4709 = CARTESIAN_POINT ( 'NONE',  ( -4.276409079477644148, -1.261996585732578335, -1.062499998634405696 ) ) ;
#4710 = CARTESIAN_POINT ( 'NONE',  ( 44.82050807568875683, -5.000000000000000000, 37.63139720814412925 ) ) ;
#4711 = CARTESIAN_POINT ( 'NONE',  ( 3.535533905932736864, -22.25000000273118417, 3.535533905932738641 ) ) ;
#4712 = ORIENTED_EDGE ( 'NONE', *, *, #1811, .F. ) ;
#4713 = CARTESIAN_POINT ( 'NONE',  ( -81.33974596215560382, -119.9999999999999716, 7.500000000000001776 ) ) ;
#4714 = ORIENTED_EDGE ( 'NONE', *, *, #11944, .F. ) ;
#4715 = FACE_OUTER_BOUND ( 'NONE', #188, .T. ) ;
#4716 = EDGE_LOOP ( 'NONE', ( #8704, #3884, #9460, #812 ) ) ;
#4717 = ORIENTED_EDGE ( 'NONE', *, *, #4623, .T. ) ;
#4718 = VECTOR ( 'NONE', #3707, 1000.000000000000000 ) ;
#4719 = VERTEX_POINT ( 'NONE', #11834 ) ;
#4720 = CARTESIAN_POINT ( 'NONE',  ( -1.261996585732579224, 4.276409079477648589, -3.312499998634407916 ) ) ;
#4721 = AXIS2_PLACEMENT_3D ( 'NONE', #11461, #11383, #7845 ) ;
#4722 = CARTESIAN_POINT ( 'NONE',  ( 0.000000000000000000, -13.00000000000000178, -1.500000000000000000 ) ) ;
#4723 = DIRECTION ( 'NONE',  ( 0.000000000000000000, 0.000000000000000000, 1.000000000000000000 ) ) ;
#4724 = CARTESIAN_POINT ( 'NONE',  ( -6.765421556309547668E-13, 50.00000000000000000, 70.14999999999929514 ) ) ;
#4725 = EDGE_CURVE ( 'NONE', #8017, #11683, #782, .T. ) ;
#4726 = CARTESIAN_POINT ( 'NONE',  ( 2.467663300281917732E-15, 50.00000000000000000, -70.14999999999999147 ) ) ;
#4727 = CARTESIAN_POINT ( 'NONE',  ( -3.401574460001764777, 4.209348295687701302, -0.5624999972688170535 ) ) ;
#4728 = CARTESIAN_POINT ( 'NONE',  ( -3.535533905932738641, -24.37500000000000000, 3.535533905932737309 ) ) ;
#4729 = CARTESIAN_POINT ( 'NONE',  ( -5.000000000000000000, -22.62500000273118772, -6.123233995736766282E-16 ) ) ;
#4730 = CARTESIAN_POINT ( 'NONE',  ( 1.846868145590735200, -24.50000000136559564, -4.458734124999999437 ) ) ;
#4731 = CARTESIAN_POINT ( 'NONE',  ( 1.261996585732578113, -4.276409079477644148, -5.562499998634406140 ) ) ;
#4732 = ORIENTED_EDGE ( 'NONE', *, *, #7757, .F. ) ;
#4733 = CARTESIAN_POINT ( 'NONE',  ( -4.336808689942017736E-16, 9.147862274876558786, -8.047472243342932430 ) ) ;
#4734 = ORIENTED_EDGE ( 'NONE', *, *, #36, .F. ) ;
#4735 = ORIENTED_EDGE ( 'NONE', *, *, #9375, .F. ) ;
#4736 =( LENGTH_UNIT ( ) NAMED_UNIT ( * ) SI_UNIT ( .MILLI., .METRE. ) );
#4737 = EDGE_LOOP ( 'NONE', ( #9222, #6497, #6815, #15565, #4308, #8587, #1852, #15680 ) ) ;
#4738 = PRODUCT_DEFINITION_SHAPE ( 'NONE', 'NONE',  #1484 ) ;
#4739 = VECTOR ( 'NONE', #13046, 1000.000000000000000 ) ;
#4740 = CARTESIAN_POINT ( 'NONE',  ( -4.458734124999999437, -22.18750000136559564, -5.460374474430324690E-16 ) ) ;
#4741 = DIRECTION ( 'NONE',  ( -0.000000000000000000, -1.000000000000000000, -0.000000000000000000 ) ) ;
#4742 = CARTESIAN_POINT ( 'NONE',  ( -120.8578643762690348, -112.8157963042559970, -17.50000000000000000 ) ) ;
#4743 = ADVANCED_FACE ( 'NONE', ( #3593 ), #10796, .T. ) ;
#4744 = CARTESIAN_POINT ( 'NONE',  ( 19.99999999999956657, -8.786575603324269439E-13, -11.50000000000000000 ) ) ;
#4745 = CARTESIAN_POINT ( 'NONE',  ( 4.896370289181508184, -4.730053418719346148, 48.48076211353311749 ) ) ;
#4746 = EDGE_CURVE ( 'NONE', #14971, #3476, #3522, .T. ) ;
#4747 = EDGE_CURVE ( 'NONE', #15077, #8700, #2369, .T. ) ;
#4748 = CARTESIAN_POINT ( 'NONE',  ( -2.886751345948139758, -37.00000000000000711, 35.00000000000000000 ) ) ;
#4749 = CARTESIAN_POINT ( 'NONE',  ( -0.5711823568785978633, -5.381735091635035495, -1.312500000000000444 ) ) ;
#4750 = CARTESIAN_POINT ( 'NONE',  ( 5.000000000000002665, 1.275685995473128912E-14, -4.045263047592942307 ) ) ;
#4751 = CARTESIAN_POINT ( 'NONE',  ( 42.02221399786069611, 2.000000000000000000, -2.649999999999884892 ) ) ;
#4752 = CARTESIAN_POINT ( 'NONE',  ( -1.846868145590734756, -30.12500000136559208, -4.458734125000000326 ) ) ;
#4753 = CARTESIAN_POINT ( 'NONE',  ( 3.753672977998667726, 3.033343224707664376, -1.499999998634408138 ) ) ;
#4754 = ORIENTED_EDGE ( 'NONE', *, *, #15220, .F. ) ;
#4755 = DIRECTION ( 'NONE',  ( 1.000000000000000000, 0.000000000000000000, 0.000000000000000000 ) ) ;
#4756 = ORIENTED_EDGE ( 'NONE', *, *, #11111, .T. ) ;
#4757 = ORIENTED_EDGE ( 'NONE', *, *, #1485, .T. ) ;
#4758 = CARTESIAN_POINT ( 'NONE',  ( -4.000000000000000888, -1.539600717839011201, -3.300726591567081591 ) ) ;
#4759 = CARTESIAN_POINT ( 'NONE',  ( -4.458734125000001214, -26.87500000136559208, 1.846868145590734089 ) ) ;
#4760 = DIRECTION ( 'NONE',  ( -0.000000000000000000, 1.000000000000000000, -0.000000000000000000 ) ) ;
#4761 = CONICAL_SURFACE ( 'NONE', #13776, 2.059999999999998721, 0.9599310885968738161 ) ;
#4762 = ORIENTED_EDGE ( 'NONE', *, *, #5244, .T. ) ;
#4763 = LINE ( 'NONE', #3543, #11243 ) ;
#4764 = DIRECTION ( 'NONE',  ( 0.000000000000000000, 0.000000000000000000, -1.000000000000000000 ) ) ;
#4765 = CARTESIAN_POINT ( 'NONE',  ( -31.74999999999995737, 5.204748896376250699E-16, -4.250000000000000000 ) ) ;
#4766 = DIRECTION ( 'NONE',  ( -1.000000000000000000, -1.541976423090495140E-16, 0.000000000000000000 ) ) ;
#4767 = EDGE_CURVE ( 'NONE', #6399, #5167, #10716, .T. ) ;
#4768 = CARTESIAN_POINT ( 'NONE',  ( -3.152801135295367985, -22.06250000136559564, 3.152801135295367096 ) ) ;
#4769 = AXIS2_PLACEMENT_3D ( 'NONE', #2354, #5759, #9801 ) ;
#4770 = LINE ( 'NONE', #7605, #14501 ) ;
#4771 = CARTESIAN_POINT ( 'NONE',  ( -5.000000000000091482, -0.7223674278660691117, -1.396799362785968501 ) ) ;
#4772 = DIRECTION ( 'NONE',  ( 0.000000000000000000, 0.000000000000000000, 1.000000000000000000 ) ) ;
#4773 = AXIS2_PLACEMENT_3D ( 'NONE', #6841, #11748, #3590 ) ;
#4774 = CARTESIAN_POINT ( 'NONE',  ( 12.67949192431126093, -35.00000000000000000, -61.96152422706632024 ) ) ;
#4775 = CARTESIAN_POINT ( 'NONE',  ( 10.00000000000098765, -13.00000000000000178, 19.82050807568871065 ) ) ;
#4776 = DIRECTION ( 'NONE',  ( 0.000000000000000000, 0.000000000000000000, 1.000000000000000000 ) ) ;
#4777 = ORIENTED_EDGE ( 'NONE', *, *, #6737, .T. ) ;
#4778 = SURFACE_STYLE_USAGE ( .BOTH. , #9702 ) ;
#4779 = ORIENTED_EDGE ( 'NONE', *, *, #3033, .T. ) ;
#4780 = CARTESIAN_POINT ( 'NONE',  ( -99.99999999999998579, -25.00000000000000711, 17.50000000000000000 ) ) ;
#4781 = VECTOR ( 'NONE', #3264, 1000.000000000000000 ) ;
#4782 = EDGE_LOOP ( 'NONE', ( #15079, #5900, #6570, #4674 ) ) ;
#4783 = CIRCLE ( 'NONE', #5813, 2.499999999999998668 ) ;
#4784 = CARTESIAN_POINT ( 'NONE',  ( -39.99999999999999289, -9.000000000000001776, 8.300651832549021947E-13 ) ) ;
#4785 = CARTESIAN_POINT ( 'NONE',  ( 4.391654775818395251, -2.390265326283149694, -3.999999997268816720 ) ) ;
#4786 = CARTESIAN_POINT ( 'NONE',  ( -4.276409079477644148, -1.261996585732578335, 0.1875000013655918341 ) ) ;
#4787 = DIRECTION ( 'NONE',  ( 0.000000000000000000, 0.000000000000000000, 1.000000000000000000 ) ) ;
#4788 =( BOUNDED_CURVE ( )  B_SPLINE_CURVE ( 2, ( #11496, #14992, #445, #3905, #10311, #6430, #15238, #2774, #291 ),
 .UNSPECIFIED., .F., .F. ) 
 B_SPLINE_CURVE_WITH_KNOTS ( ( 3, 2, 2, 2, 3 ),
 ( 0.2249999999999998668, 0.2374999999999998501, 0.2499999999999998890, 0.2624999999999999001, 0.2749999999999999112 ),
 .UNSPECIFIED. ) 
 CURVE ( )  GEOMETRIC_REPRESENTATION_ITEM ( )  RATIONAL_B_SPLINE_CURVE ( ( 1.000000000000000888, 0.9238795325112858503, 1.000000000000000000, 0.9238795325112867385, 1.000000000000000000, 0.9238795325112867385, 1.000000000000000000, 0.9238795325112874046, 0.9999999999999993339 ) ) 
 REPRESENTATION_ITEM ( '' )  );
#4789 = AXIS2_PLACEMENT_3D ( 'NONE', #965, #5892, #6135 ) ;
#4790 = CARTESIAN_POINT ( 'NONE',  ( -3.753672977998669946, -3.033343224707661712, -2.999999998634409248 ) ) ;
#4791 = PLANE ( 'NONE',  #14105 ) ;
#4792 = CARTESIAN_POINT ( 'NONE',  ( 0.6920835326022565237, 4.454600218803884459, -3.597382984111579862 ) ) ;
#4793 = VERTEX_POINT ( 'NONE', #15885 ) ;
#4794 = CARTESIAN_POINT ( 'NONE',  ( 4.896370289192182312, -5.000000000000000000, -48.48076211352908871 ) ) ;
#4795 =( NAMED_UNIT ( * ) SI_UNIT ( $, .STERADIAN. ) SOLID_ANGLE_UNIT ( ) );
#4796 = ORIENTED_EDGE ( 'NONE', *, *, #1126, .T. ) ;
#4797 = SPHERICAL_SURFACE ( 'NONE', #9295, 10.00000000000000000 ) ;
#4798 = DIRECTION ( 'NONE',  ( -0.000000000000000000, -1.000000000000000000, -0.000000000000000000 ) ) ;
#4799 = ORIENTED_EDGE ( 'NONE', *, *, #5413, .T. ) ;
#4800 = CARTESIAN_POINT ( 'NONE',  ( -2.131511515620587272, -3.916244202832140253, -3.937499998634408360 ) ) ;
#4801 = EDGE_CURVE ( 'NONE', #7835, #8282, #14633, .T. ) ;
#4802 = ADVANCED_FACE ( 'NONE', ( #3357 ), #15650, .T. ) ;
#4803 = VECTOR ( 'NONE', #13537, 1000.000000000000227 ) ;
#4804 = CARTESIAN_POINT ( 'NONE',  ( 0.000000000000000000, -11.00000000000000178, 0.000000000000000000 ) ) ;
#4805 = AXIS2_PLACEMENT_3D ( 'NONE', #1677, #8808, #3941 ) ;
#4806 = CARTESIAN_POINT ( 'NONE',  ( -35.00000000000000000, 40.00000000000000000, 0.000000000000000000 ) ) ;
#4807 = CARTESIAN_POINT ( 'NONE',  ( -7.894787914004613327, -1.222495057920810896E-13, -7.591390474663425536 ) ) ;
#4808 = CARTESIAN_POINT ( 'NONE',  ( 47.32050807568875683, -4.999999999999997335, 41.96152422706633445 ) ) ;
#4809 = FACE_OUTER_BOUND ( 'NONE', #15645, .T. ) ;
#4810 = CARTESIAN_POINT ( 'NONE',  ( 0.5711823568785989735, 5.381735091635026613, 0.3125000027311818918 ) ) ;
#4811 = SURFACE_STYLE_USAGE ( .BOTH. , #13363 ) ;
#4812 = AXIS2_PLACEMENT_3D ( 'NONE', #8675, #2507, #2594 ) ;
#4813 =( LENGTH_UNIT ( ) NAMED_UNIT ( * ) SI_UNIT ( .MILLI., .METRE. ) );
#4814 = CARTESIAN_POINT ( 'NONE',  ( -3.152801135295367096, -27.31250000136559564, -3.152801135295367541 ) ) ;
#4815 = CARTESIAN_POINT ( 'NONE',  ( -0.5093500532425060401, -4.799145180956616130, -5.624999998634406140 ) ) ;
#4816 = DIRECTION ( 'NONE',  ( -0.8660254037844387076, 0.000000000000000000, 0.4999999999999998335 ) ) ;
#4817 = VERTEX_POINT ( 'NONE', #1159 ) ;
#4818 = ORIENTED_EDGE ( 'NONE', *, *, #6863, .T. ) ;
#4819 = ORIENTED_EDGE ( 'NONE', *, *, #3722, .T. ) ;
#4820 = CARTESIAN_POINT ( 'NONE',  ( -4.458734125000000326, -22.25000000136559564, -1.846868145590735644 ) ) ;
#4821 = EDGE_CURVE ( 'NONE', #3191, #6800, #5082, .T. ) ;
#4822 = DIRECTION ( 'NONE',  ( 0.000000000000000000, 0.000000000000000000, -1.000000000000000000 ) ) ;
#4823 = ADVANCED_FACE ( 'NONE', ( #2441 ), #13429, .T. ) ;
#4824 = PRODUCT_DEFINITION ( 'UNKNOWN', '', #1989, #295 ) ;
#4825 = CARTESIAN_POINT ( 'NONE',  ( 0.000000000000000000, 0.000000000000000000, -25.03750572909317285 ) ) ;
#4826 = AXIS2_PLACEMENT_3D ( 'NONE', #954, #10884, #5882 ) ;
#4827 = CARTESIAN_POINT ( 'NONE',  ( 19.99999999999956657, -8.786575603324269439E-13, -11.50000000000000000 ) ) ;
#4828 = DIRECTION ( 'NONE',  ( 0.000000000000000000, 0.000000000000000000, 1.000000000000000000 ) ) ;
#4829 = CARTESIAN_POINT ( 'NONE',  ( 42.02221399786069611, 0.000000000000000000, -2.649999999999888445 ) ) ;
#4830 = LINE ( 'NONE', #11929, #7736 ) ;
#4831 = CARTESIAN_POINT ( 'NONE',  ( -4.209348295687703967, -3.401574460001763001, -1.437500000000001998 ) ) ;
#4832 = DIRECTION ( 'NONE',  ( 1.000000000000000000, 0.000000000000000000, 0.000000000000000000 ) ) ;
#4833 = LINE ( 'NONE', #2239, #12845 ) ;
#4834 = CARTESIAN_POINT ( 'NONE',  ( -4.458734125000001214, -27.87500000136559564, 1.846868145590734089 ) ) ;
#4835 = CARTESIAN_POINT ( 'NONE',  ( -4.799145180956616130, 0.5093500532425063732, -1.124999998634405918 ) ) ;
#4836 = ORIENTED_EDGE ( 'NONE', *, *, #1072, .T. ) ;
#4837 = CARTESIAN_POINT ( 'NONE',  ( 35.00000000000000000, 37.00000000000000000, 2.649999999999976819 ) ) ;
#4838 = ORIENTED_EDGE ( 'NONE', *, *, #9269, .F. ) ;
#4839 = AXIS2_PLACEMENT_3D ( 'NONE', #3044, #7990, #706 ) ;
#4840 = ORIENTED_EDGE ( 'NONE', *, *, #13923, .F. ) ;
#4841 = FACE_OUTER_BOUND ( 'NONE', #13689, .T. ) ;
#4842 = APPLICATION_CONTEXT ( 'automotive_design' ) ;
#4843 = CARTESIAN_POINT ( 'NONE',  ( -3.152801135295367096, -25.06250000136559564, -3.152801135295367541 ) ) ;
#4844 = ADVANCED_FACE ( 'NONE', ( #6101 ), #4568, .F. ) ;
#4845 = CARTESIAN_POINT ( 'NONE',  ( -31.74999999999995737, 0.000000000000000000, 0.000000000000000000 ) ) ;
#4846 = EDGE_CURVE ( 'NONE', #15819, #9634, #856, .T. ) ;
#4847 = EDGE_LOOP ( 'NONE', ( #3938, #9513, #6010, #14921, #1131, #12632 ) ) ;
#4848 = CIRCLE ( 'NONE', #2502, 2.649999999999992806 ) ;
#4849 = FACE_BOUND ( 'NONE', #7910, .T. ) ;
#4851 = VECTOR ( 'NONE', #15912, 1000.000000000000000 ) ;
#4850 = CARTESIAN_POINT ( 'NONE',  ( -28.86751345948126257, -4.999999999999997335, -50.00000000000000711 ) ) ;
#4852 = CARTESIAN_POINT ( 'NONE',  ( 4.000000000000000000, 2.309401076758497151, -3.433295621305379353 ) ) ;
#4853 = FACE_BOUND ( 'NONE', #166, .T. ) ;
#4854 = CARTESIAN_POINT ( 'NONE',  ( 1.846868145590735200, -22.50000000136559208, -4.458734125000000326 ) ) ;
#4855 = FACE_OUTER_BOUND ( 'NONE', #2311, .T. ) ;
#4856 = CARTESIAN_POINT ( 'NONE',  ( 44.82050807568875683, 0.000000000000000000, 37.63139720814412925 ) ) ;
#4857 = CARTESIAN_POINT ( 'NONE',  ( -9.184850993605147944E-16, -29.37500000273118417, 5.000000000000000000 ) ) ;
#4858 = DIRECTION ( 'NONE',  ( 0.000000000000000000, 0.000000000000000000, 1.000000000000000000 ) ) ;
#4859 = VECTOR ( 'NONE', #1000, 1000.000000000000000 ) ;
#4860 = DIRECTION ( 'NONE',  ( -0.000000000000000000, -1.000000000000000000, -0.000000000000000000 ) ) ;
#4861 = DIRECTION ( 'NONE',  ( -0.000000000000000000, 1.000000000000000000, -0.000000000000000000 ) ) ;
#4862 = EDGE_LOOP ( 'NONE', ( #9433, #4374, #9993, #8827 ) ) ;
#4863 = CIRCLE ( 'NONE', #13098, 25.00000000000000000 ) ;
#4864 = EDGE_LOOP ( 'NONE', ( #8155, #13074, #2811, #5258 ) ) ;
#4865 = LINE ( 'NONE', #14798, #4531 ) ;
#4866 = CIRCLE ( 'NONE', #15198, 2.500000000000909495 ) ;
#4867 = EDGE_CURVE ( 'NONE', #7219, #3541, #15551, .T. ) ;
#4868 = ORIENTED_EDGE ( 'NONE', *, *, #15495, .F. ) ;
#4869 = CARTESIAN_POINT ( 'NONE',  ( 0.000000000000000000, -1.178949249685213863, 2.042000000000002924 ) ) ;
#4870 = AXIS2_PLACEMENT_3D ( 'NONE', #11110, #14829, #15741 ) ;
#4871 = AXIS2_PLACEMENT_3D ( 'NONE', #4316, #3107, #764 ) ;
#4872 = CARTESIAN_POINT ( 'NONE',  ( -3.535533905932738641, -25.50000000273118417, 3.535533905932737309 ) ) ;
#4873 = CARTESIAN_POINT ( 'NONE',  ( -0.5093500532425060401, -4.799145180956616130, 0.3750000013655915843 ) ) ;
#4874 = CIRCLE ( 'NONE', #9271, 2.100000000000000089 ) ;
#4875 = DIRECTION ( 'NONE',  ( 6.123233995736766036E-17, 1.000000000000000000, 0.000000000000000000 ) ) ;
#4876 = AXIS2_PLACEMENT_3D ( 'NONE', #14709, #3630, #11075 ) ;
#4877 = CARTESIAN_POINT ( 'NONE',  ( -3.916244202832140253, 2.131511515620587272, -1.187499998634405918 ) ) ;
#4878 = DIRECTION ( 'NONE',  ( 1.000000000000000000, 0.000000000000000000, 0.000000000000000000 ) ) ;
#4879 = CARTESIAN_POINT ( 'NONE',  ( 0.000000000000000000, 0.000000000000000000, 0.000000000000000000 ) ) ;
#4880 = VERTEX_POINT ( 'NONE', #2299 ) ;
#4881 = CARTESIAN_POINT ( 'NONE',  ( 9.184850993605153466E-15, 40.00000000000000000, 75.00000000000004263 ) ) ;
#4882 = EDGE_LOOP ( 'NONE', ( #9583, #6616, #2038 ) ) ;
#4883 = EDGE_LOOP ( 'NONE', ( #8058, #11186, #2909, #9567 ) ) ;
#4884 = CARTESIAN_POINT ( 'NONE',  ( -0.5093500532425060401, -4.799145180956616130, -1.874999998634406584 ) ) ;
#4885 = CARTESIAN_POINT ( 'NONE',  ( 4.000000000000000000, 0.000000000000000000, 0.000000000000000000 ) ) ;
#4886 = VECTOR ( 'NONE', #6814, 1000.000000000000114 ) ;
#4887 =( BOUNDED_CURVE ( )  B_SPLINE_CURVE ( 2, ( #4297, #8915, #13819, #2754, #351, #14162, #7863, #7711, #7621 ),
 .UNSPECIFIED., .F., .F. ) 
 B_SPLINE_CURVE_WITH_KNOTS ( ( 3, 2, 2, 2, 3 ),
 ( 0.02500000000000002220, 0.03750000000000003331, 0.05000000000000004441, 0.06250000000000005551, 0.07500000000000006661 ),
 .UNSPECIFIED. ) 
 CURVE ( )  GEOMETRIC_REPRESENTATION_ITEM ( )  RATIONAL_B_SPLINE_CURVE ( ( 0.9999999999999998890, 0.9238795325112868495, 1.000000000000000000, 0.9238795325112867385, 1.000000000000000000, 0.9238795325112867385, 1.000000000000000000, 0.9238795325112862944, 1.000000000000000444 ) ) 
 REPRESENTATION_ITEM ( '' )  );
#4888 = CARTESIAN_POINT ( 'NONE',  ( 2.500000000000000000, -1.178949249685218303, -2.041999999999998039 ) ) ;
#4889 = CARTESIAN_POINT ( 'NONE',  ( 0.000000000000000000, 37.00000000000000000, 0.000000000000000000 ) ) ;
#4890 = DIRECTION ( 'NONE',  ( 0.000000000000000000, 0.000000000000000000, -1.000000000000000000 ) ) ;
#4891 = CARTESIAN_POINT ( 'NONE',  ( -4.209348295687703967, -3.401574460001763001, -1.312499997268813834 ) ) ;
#4892 = CARTESIAN_POINT ( 'NONE',  ( 45.58845726811988897, -35.00000000000000000, 42.96152422706634155 ) ) ;
#4893 = EDGE_CURVE ( 'NONE', #928, #8391, #4059, .T. ) ;
#4894 = CARTESIAN_POINT ( 'NONE',  ( -116.3391301858327296, -120.2076149402627294, 17.50000000000000000 ) ) ;
#4895 = CARTESIAN_POINT ( 'NONE',  ( 4.458734124999999437, -26.68750000136559564, 0.000000000000000000 ) ) ;
#4896 = CARTESIAN_POINT ( 'NONE',  ( -1.846868145590734756, -22.12500000136559564, -4.458734124999999437 ) ) ;
#4897 = CARTESIAN_POINT ( 'NONE',  ( 0.5093500532425063732, 4.799145180956616130, -3.124999998634407916 ) ) ;
#4898 = CARTESIAN_POINT ( 'NONE',  ( 45.58845726811991739, -35.00000000000000000, -42.96152422706631313 ) ) ;
#4899 = ORIENTED_EDGE ( 'NONE', *, *, #5361, .F. ) ;
#4900 = ORIENTED_EDGE ( 'NONE', *, *, #13733, .T. ) ;
#4901 = DIRECTION ( 'NONE',  ( 0.000000000000000000, 0.000000000000000000, 1.000000000000000000 ) ) ;
#4902 = EDGE_LOOP ( 'NONE', ( #6854, #14386 ) ) ;
#4903 = CARTESIAN_POINT ( 'NONE',  ( -8.190561711645485556E-16, -24.93750000136559564, 4.458734124999999437 ) ) ;
#4904 = FACE_OUTER_BOUND ( 'NONE', #6076, .T. ) ;
#4905 = DIRECTION ( 'NONE',  ( 1.000000000000000000, 0.000000000000000000, 0.000000000000000000 ) ) ;
#4906 = DIRECTION ( 'NONE',  ( 0.000000000000000000, 0.000000000000000000, -1.000000000000000000 ) ) ;
#4907 = FACE_BOUND ( 'NONE', #8075, .T. ) ;
#4908 = CARTESIAN_POINT ( 'NONE',  ( -28.86751345948126257, 1.999999999999998224, -50.00000000000000711 ) ) ;
#4909 = CARTESIAN_POINT ( 'NONE',  ( -4.795541693661363958, -1.415196051561583790, 0.4999999999999970024 ) ) ;
#4910 = EDGE_CURVE ( 'NONE', #4992, #11474, #1082, .T. ) ;
#4911 = CARTESIAN_POINT ( 'NONE',  ( 2.971083655575039728, -3.963652976736657507, -0.03751319233342364362 ) ) ;
#4912 = EDGE_CURVE ( 'NONE', #10893, #3787, #8460, .T. ) ;
#4913 = CARTESIAN_POINT ( 'NONE',  ( -4.458734124999999437, -25.93750000136559564, -5.460374474430324690E-16 ) ) ;
#4914 = CARTESIAN_POINT ( 'NONE',  ( -2.131511515620587272, -3.916244202832140253, -3.937499998634408360 ) ) ;
#4915 = VERTEX_POINT ( 'NONE', #13270 ) ;
#4916 = CARTESIAN_POINT ( 'NONE',  ( -7.500000000000007105, -0.7512838658081422150, -2.971391578968086378E-15 ) ) ;
#4917 = ORIENTED_EDGE ( 'NONE', *, *, #6093, .F. ) ;
#4918 = ORIENTED_EDGE ( 'NONE', *, *, #7113, .T. ) ;
#4919 = CARTESIAN_POINT ( 'NONE',  ( -7.500000000000003553, -3.948305025207483610, -7.349903712355165375 ) ) ;
#4920 = CARTESIAN_POINT ( 'NONE',  ( 3.152801135295367541, -23.31250000136559564, -3.152801135295367541 ) ) ;
#4921 = CARTESIAN_POINT ( 'NONE',  ( 67.49999999999931788, 50.00000000000000000, 2.650000000000006573 ) ) ;
#4922 = STYLED_ITEM ( 'NONE', ( #6909 ), #3697 ) ;
#4923 = EDGE_LOOP ( 'NONE', ( #8098, #8858 ) ) ;
#4924 = LINE ( 'NONE', #11072, #8137 ) ;
#4925 = DIRECTION ( 'NONE',  ( 0.000000000000000000, 0.000000000000000000, 1.000000000000000000 ) ) ;
#4926 = LINE ( 'NONE', #6150, #11051 ) ;
#4927 = LINE ( 'NONE', #10907, #15566 ) ;
#4928 = CARTESIAN_POINT ( 'NONE',  ( -1.846868145590734756, -25.37500000136559919, -4.458734125000000326 ) ) ;
#4929 = CARTESIAN_POINT ( 'NONE',  ( 43.08845726811987475, 0.000000000000000000, 38.63139720814412925 ) ) ;
#4930 = EDGE_CURVE ( 'NONE', #6800, #3191, #203, .T. ) ;
#4931 = CYLINDRICAL_SURFACE ( 'NONE', #3084, 5.000000000000000888 ) ;
#4932 = ADVANCED_FACE ( 'NONE', ( #9645 ), #14667, .F. ) ;
#4933 = CARTESIAN_POINT ( 'NONE',  ( -2.071067811865478170, -28.43750000273119127, 5.000000000000000000 ) ) ;
#4934 = CARTESIAN_POINT ( 'NONE',  ( 12.67949192431120586, -37.00000000000000711, 61.96152422706632024 ) ) ;
#4935 = CARTESIAN_POINT ( 'NONE',  ( 1.846868145590735200, -29.25000000136559564, -4.458734124999999437 ) ) ;
#4936 = FACE_OUTER_BOUND ( 'NONE', #11450, .T. ) ;
#4937 = ORIENTED_EDGE ( 'NONE', *, *, #6643, .T. ) ;
#4938 = PRODUCT_DEFINITION_SHAPE ( 'NONE', 'NONE',  #15996 ) ;
#4939 = ORIENTED_EDGE ( 'NONE', *, *, #8923, .T. ) ;
#4940 = CARTESIAN_POINT ( 'NONE',  ( 0.000000000000000000, 2.357898499370433054, -1.951563910473907981E-15 ) ) ;
#4941 = ORIENTED_EDGE ( 'NONE', *, *, #13234, .T. ) ;
#4942 = DIRECTION ( 'NONE',  ( -1.000000000000000000, -0.000000000000000000, -0.000000000000000000 ) ) ;
#4943 = CARTESIAN_POINT ( 'NONE',  ( 40.79973832332031236, -3.012258285427884541, 27.17844299114864626 ) ) ;
#4944 = EDGE_CURVE ( 'NONE', #15162, #10748, #8209, .T. ) ;
#4945 = CARTESIAN_POINT ( 'NONE',  ( -1.261996585732579224, 4.276409079477648589, -3.062499998634407472 ) ) ;
#4946 = APPLICATION_PROTOCOL_DEFINITION ( 'draft international standard', 'automotive_design', 1998, #723 ) ;
#4947 = EDGE_CURVE ( 'NONE', #74, #4219, #10273, .T. ) ;
#4948 = CARTESIAN_POINT ( 'NONE',  ( -3.753672977998669946, -3.033343224707661712, -3.999999998634410137 ) ) ;
#4949 = CARTESIAN_POINT ( 'NONE',  ( -94.99999999999995737, -103.6602540378443962, -7.500000000000000000 ) ) ;
#4950 = LINE ( 'NONE', #3580, #7713 ) ;
#4951 =( REPRESENTATION_RELATIONSHIP ('NONE','NONE', #4176, #4696 ) REPRESENTATION_RELATIONSHIP_WITH_TRANSFORMATION ( #3900 )SHAPE_REPRESENTATION_RELATIONSHIP( ) );
#4952 = ORIENTED_EDGE ( 'NONE', *, *, #11708, .F. ) ;
#4953 = FACE_OUTER_BOUND ( 'NONE', #10077, .T. ) ;
#4954 = CYLINDRICAL_SURFACE ( 'NONE', #8447, 2.499999999999998668 ) ;
#4955 = ORIENTED_EDGE ( 'NONE', *, *, #14391, .F. ) ;
#4956 = CARTESIAN_POINT ( 'NONE',  ( 2.131511515620586383, 3.916244202832140253, -4.437499998634405252 ) ) ;
#4957 = FACE_OUTER_BOUND ( 'NONE', #12642, .T. ) ;
#4958 = CARTESIAN_POINT ( 'NONE',  ( 24.55500000000002103, 0.000000000000000000, 0.000000000000000000 ) ) ;
#4959 = CARTESIAN_POINT ( 'NONE',  ( -1.154700538379222596, 88.59290746114278647, -34.00000000000000000 ) ) ;
#4960 = CARTESIAN_POINT ( 'NONE',  ( -4.795541693661363958, -1.415196051561583790, -2.500000000000002220 ) ) ;
#4961 = UNCERTAINTY_MEASURE_WITH_UNIT (LENGTH_MEASURE( 1.000000000000000082E-05 ), #4539, 'distance_accuracy_value', 'NONE');
#4962 = ADVANCED_FACE ( 'NONE', ( #14913 ), #2610, .F. ) ;
#4963 = DIRECTION ( 'NONE',  ( -1.000000000000000000, 0.000000000000000000, 0.000000000000000000 ) ) ;
#4964 = CARTESIAN_POINT ( 'NONE',  ( 4.391654775818395251, -2.390265326283149694, 1.000000002731184168 ) ) ;
#4965 = CARTESIAN_POINT ( 'NONE',  ( 9.999999999999891642, -13.00000000000000178, -14.82050807568883677 ) ) ;
#4966 = CARTESIAN_POINT ( 'NONE',  ( -4.081282237088195153, 2.167655003740347475, -0.2732678705139793274 ) ) ;
#4967 = CARTESIAN_POINT ( 'NONE',  ( -3.152801135295367096, -26.31250000136559564, -3.152801135295367541 ) ) ;
#4968 = CARTESIAN_POINT ( 'NONE',  ( 1.846868145590736310, -21.62500000136559208, 4.458734124999997661 ) ) ;
#4969 = CARTESIAN_POINT ( 'NONE',  ( 4.276409079477644148, 1.261996585732577891, -3.312499998634407916 ) ) ;
#4970 = DIRECTION ( 'NONE',  ( 0.000000000000000000, -1.000000000000000000, 0.000000000000000000 ) ) ;
#4971 = ORIENTED_EDGE ( 'NONE', *, *, #2238, .F. ) ;
#4972 = ORIENTED_EDGE ( 'NONE', *, *, #13283, .T. ) ;
#4973 = DIRECTION ( 'NONE',  ( 0.8660254037844432595, 0.000000000000000000, -0.4999999999999919509 ) ) ;
#4974 = ORIENTED_EDGE ( 'NONE', *, *, #4999, .F. ) ;
#4975 = CARTESIAN_POINT ( 'NONE',  ( -4.458734125000001214, -23.12500000136559564, 1.846868145590734089 ) ) ;
#4976 = EDGE_CURVE ( 'NONE', #12106, #10564, #3297, .T. ) ;
#4977 = DIRECTION ( 'NONE',  ( 0.000000000000000000, -0.000000000000000000, 1.000000000000000000 ) ) ;
#4978 = PLANE ( 'NONE',  #13512 ) ;
#4979 = VECTOR ( 'NONE', #12485, 1000.000000000000000 ) ;
#4980 = EDGE_CURVE ( 'NONE', #3993, #11064, #1219, .T. ) ;
#4981 = AXIS2_PLACEMENT_3D ( 'NONE', #8139, #7002, #6837 ) ;
#4982 = CARTESIAN_POINT ( 'NONE',  ( 6.000000000000000000, -20.00000000000000000, 1.500000000000000000 ) ) ;
#4983 = CARTESIAN_POINT ( 'NONE',  ( 4.391654732552941809, -2.390265405775130692, 0.000000000000000000 ) ) ;
#4984 = CARTESIAN_POINT ( 'NONE',  ( -17.99999999999979394, -9.000000000000001776, -3.500000000000000888 ) ) ;
#4985 = CARTESIAN_POINT ( 'NONE',  ( 1.415196051561583790, -4.795541693661363958, -1.250000000000001110 ) ) ;
#4986 = DIRECTION ( 'NONE',  ( 0.000000000000000000, 1.000000000000000000, 0.000000000000000000 ) ) ;
#4987 = LINE ( 'NONE', #2879, #15459 ) ;
#4988 = CARTESIAN_POINT ( 'NONE',  ( -8.190561711645485556E-16, -28.68750000136559564, 4.458734124999999437 ) ) ;
#4989 = CARTESIAN_POINT ( 'NONE',  ( -3.033343224707664376, 3.753672977998667726, -4.249999998634406140 ) ) ;
#4990 = ORIENTED_EDGE ( 'NONE', *, *, #6750, .F. ) ;
#4991 = CYLINDRICAL_SURFACE ( 'NONE', #2719, 2.649999999999992806 ) ;
#4992 = VERTEX_POINT ( 'NONE', #4068 ) ;
#4993 = VERTEX_POINT ( 'NONE', #14823 ) ;
#4994 = FACE_OUTER_BOUND ( 'NONE', #1406, .T. ) ;
#4995 = CARTESIAN_POINT ( 'NONE',  ( 4.458734124999999437, -24.50000000136559564, 1.846868145590737864 ) ) ;
#4996 = CARTESIAN_POINT ( 'NONE',  ( -28.86751345948126612, -5.000000000000000000, -22.00000000000000711 ) ) ;
#4997 = EDGE_LOOP ( 'NONE', ( #10338, #14838, #5170, #4840, #10897, #15620, #7765, #2828 ) ) ;
#4998 = DIRECTION ( 'NONE',  ( -0.8660254037844405950, 0.4999999999999965028, 0.000000000000000000 ) ) ;
#4999 = EDGE_CURVE ( 'NONE', #14811, #10919, #14396, .T. ) ;
#5000 = EDGE_CURVE ( 'NONE', #12993, #742, #5132, .T. ) ;
#5001 = CARTESIAN_POINT ( 'NONE',  ( 0.000000000000000000, -20.00000000000000000, 0.000000000000000000 ) ) ;
#5002 = DIRECTION ( 'NONE',  ( -0.000000000000000000, -0.000000000000000000, -1.000000000000000000 ) ) ;
#5003 = CARTESIAN_POINT ( 'NONE',  ( 0.000000000000000000, -20.00000000000000000, 0.000000000000000000 ) ) ;
#5004 = CARTESIAN_POINT ( 'NONE',  ( -9.184850993605147944E-16, -30.25000000000000000, 5.000000000000000000 ) ) ;
#5005 = CARTESIAN_POINT ( 'NONE',  ( 0.000000000000000000, 0.000000000000000000, -5.000000000000000888 ) ) ;
#5006 = DIRECTION ( 'NONE',  ( 1.000000000000000000, 0.000000000000000000, 0.000000000000000000 ) ) ;
#5007 = CARTESIAN_POINT ( 'NONE',  ( -5.000000000000000888, -29.56250000273118417, 2.071067811865474617 ) ) ;
#5008 = CARTESIAN_POINT ( 'NONE',  ( 3.753672977998667726, 3.033343224707664820, -8.499999998634411469 ) ) ;
#5009 = STYLED_ITEM ( 'NONE', ( #4662 ), #5806 ) ;
#5010 = CARTESIAN_POINT ( 'NONE',  ( 4.458734124999997661, -28.50000000136559564, 1.846868145590737864 ) ) ;
#5011 = FILL_AREA_STYLE_COLOUR ( '', #7644 ) ;
#5012 = ORIENTED_EDGE ( 'NONE', *, *, #10875, .T. ) ;
#5013 = TOROIDAL_SURFACE ( 'NONE', #4241, 5.384454397937118664, 0.5155456020628804703 ) ;
#5014 =( NAMED_UNIT ( * ) SI_UNIT ( $, .STERADIAN. ) SOLID_ANGLE_UNIT ( ) );
#5015 = ORIENTED_EDGE ( 'NONE', *, *, #9686, .F. ) ;
#5016 = DIRECTION ( 'NONE',  ( 0.000000000000000000, 1.000000000000000000, -0.000000000000000000 ) ) ;
#5017 = ORIENTED_EDGE ( 'NONE', *, *, #4944, .T. ) ;
#5018 = CARTESIAN_POINT ( 'NONE',  ( 0.000000000000000000, -1.178949249685218303, -2.041999999999998039 ) ) ;
#5019 = EDGE_CURVE ( 'NONE', #4014, #7371, #6431, .T. ) ;
#5020 = PRODUCT_DEFINITION ( 'UNKNOWN', '', #5348, #15314 ) ;
#5021 = CIRCLE ( 'NONE', #7622, 32.00000000000000711 ) ;
#5022 = LINE ( 'NONE', #13484, #3835 ) ;
#5023 = CARTESIAN_POINT ( 'NONE',  ( -3.753672977998669946, -3.033343224707661712, -3.749999998634409692 ) ) ;
#5024 = APPLICATION_PROTOCOL_DEFINITION ( 'draft international standard', 'automotive_design', 1998, #12774 ) ;
#5025 = CARTESIAN_POINT ( 'NONE',  ( -3.033343224707664376, 3.753672977998667726, -5.249999998634407028 ) ) ;
#5026 = FACE_OUTER_BOUND ( 'NONE', #7020, .T. ) ;
#5027 = CARTESIAN_POINT ( 'NONE',  ( 5.000000000000000000, -24.00000000000000000, 0.000000000000000000 ) ) ;
#5028 = ORIENTED_EDGE ( 'NONE', *, *, #4051, .T. ) ;
#5029 =( GEOMETRIC_REPRESENTATION_CONTEXT ( 3 ) GLOBAL_UNCERTAINTY_ASSIGNED_CONTEXT ( ( #12385 ) ) GLOBAL_UNIT_ASSIGNED_CONTEXT ( ( #2512, #2289, #2598 ) ) REPRESENTATION_CONTEXT ( 'NONE', 'WORKASPACE' ) );
#5030 = DIRECTION ( 'NONE',  ( -0.000000000000000000, 1.000000000000000000, -0.000000000000000000 ) ) ;
#5031 = AXIS2_PLACEMENT_3D ( 'NONE', #6754, #9334, #769 ) ;
#5032 =( LENGTH_UNIT ( ) NAMED_UNIT ( * ) SI_UNIT ( .MILLI., .METRE. ) );
#5033 = ORIENTED_EDGE ( 'NONE', *, *, #11796, .F. ) ;
#5034 = DIRECTION ( 'NONE',  ( 1.000000000000000000, 0.000000000000000000, -1.387778780781446464E-15 ) ) ;
#5035 = DIRECTION ( 'NONE',  ( 0.000000000000000000, 0.000000000000000000, 1.000000000000000000 ) ) ;
#5036 = AXIS2_PLACEMENT_3D ( 'NONE', #4784, #5756, #7297 ) ;
#5037 = ORIENTED_EDGE ( 'NONE', *, *, #8486, .F. ) ;
#5038 = CARTESIAN_POINT ( 'NONE',  ( -4.276409079477644148, -1.261996585732578335, -2.062499998634406584 ) ) ;
#5039 = ADVANCED_FACE ( 'NONE', ( #13844 ), #2525, .F. ) ;
#5040 = ADVANCED_FACE ( 'NONE', ( #12303 ), #12626, .T. ) ;
#5041 = EDGE_CURVE ( 'NONE', #2454, #5622, #14763, .T. ) ;
#5042 = DIRECTION ( 'NONE',  ( -0.5000000000000005551, 0.000000000000000000, 0.8660254037844382635 ) ) ;
#5043 = CARTESIAN_POINT ( 'NONE',  ( -2.171643655288372443, 3.365003104552320767, 2.541098841762897165E-18 ) ) ;
#5044 = DIRECTION ( 'NONE',  ( -0.000000000000000000, 1.000000000000000000, -0.000000000000000000 ) ) ;
#5045 = VECTOR ( 'NONE', #13460, 1000.000000000000000 ) ;
#5046 = CARTESIAN_POINT ( 'NONE',  ( 5.000000000000000000, -27.12500000273118772, 0.000000000000000000 ) ) ;
#5047 = CARTESIAN_POINT ( 'NONE',  ( -5.381735091635034607, 0.5711823568785950878, -4.437499997268819385 ) ) ;
#5048 = CARTESIAN_POINT ( 'NONE',  ( -81.39906451651640396, -110.0001759360922051, 17.50000000000000000 ) ) ;
#5049 = FACE_OUTER_BOUND ( 'NONE', #14235, .T. ) ;
#5050 = CARTESIAN_POINT ( 'NONE',  ( -3.152801135295367985, -27.06250000136559564, 3.152801135295367096 ) ) ;
#5051 = ORIENTED_EDGE ( 'NONE', *, *, #2929, .T. ) ;
#5052 = FACE_OUTER_BOUND ( 'NONE', #5584, .T. ) ;
#5053 = CARTESIAN_POINT ( 'NONE',  ( -4.276409079477644148, -1.261996585732578335, -2.812499998634407472 ) ) ;
#5054 = CARTESIAN_POINT ( 'NONE',  ( -2.688821387764050996E-14, -4.618802153517012954, -0.4999999999999995559 ) ) ;
#5055 = ORIENTED_EDGE ( 'NONE', *, *, #8996, .F. ) ;
#5056 = ORIENTED_EDGE ( 'NONE', *, *, #11652, .F. ) ;
#5057 = AXIS2_PLACEMENT_3D ( 'NONE', #8786, #6275, #134 ) ;
#5058 = ORIENTED_EDGE ( 'NONE', *, *, #14714, .F. ) ;
#5059 = CARTESIAN_POINT ( 'NONE',  ( -8.190561711645485556E-16, -23.93750000136559564, 4.458734124999999437 ) ) ;
#5060 = LINE ( 'NONE', #9996, #6116 ) ;
#5061 = VECTOR ( 'NONE', #4430, 1000.000000000000000 ) ;
#5062 = EDGE_CURVE ( 'NONE', #12678, #74, #45, .T. ) ;
#5063 = DIRECTION ( 'NONE',  ( 0.000000000000000000, 1.000000000000000000, 0.000000000000000000 ) ) ;
#5064 = LINE ( 'NONE', #2798, #5351 ) ;
#5066 = CARTESIAN_POINT ( 'NONE',  ( -5.000000000000015987, 5.773502691896279515, -7.063244554130010400 ) ) ;
#5065 = VECTOR ( 'NONE', #11504, 1000.000000000000000 ) ;
#5067 = DIRECTION ( 'NONE',  ( -0.5000000000000005551, 0.000000000000000000, 0.8660254037844382635 ) ) ;
#5068 = PRODUCT_DEFINITION_SHAPE ( 'NONE', 'NONE',  #15981 ) ;
#5069 = CARTESIAN_POINT ( 'NONE',  ( 0.5711823568785989735, 5.381735091635026613, -3.812499999999998668 ) ) ;
#5070 = DIRECTION ( 'NONE',  ( -0.000000000000000000, -0.000000000000000000, 1.000000000000000000 ) ) ;
#5071 = FACE_BOUND ( 'NONE', #9706, .T. ) ;
#5072 = CARTESIAN_POINT ( 'NONE',  ( -4.458734125000000326, -25.00000000136559564, -1.846868145590735644 ) ) ;
#5073 = AXIS2_PLACEMENT_3D ( 'NONE', #2870, #2705, #7663 ) ;
#5074 = CARTESIAN_POINT ( 'NONE',  ( 4.276409079477644148, 1.261996585732577891, -4.562499998634405252 ) ) ;
#5075 = ORIENTED_EDGE ( 'NONE', *, *, #5320, .T. ) ;
#5076 = DIRECTION ( 'NONE',  ( -0.000000000000000000, -1.000000000000000000, 0.000000000000000000 ) ) ;
#5077 = EDGE_LOOP ( 'NONE', ( #890, #9771, #11022, #8340 ) ) ;
#5078 = EDGE_LOOP ( 'NONE', ( #5037, #9987, #4732, #5385, #4370, #12821, #9419, #3385 ) ) ;
#5079 = DIRECTION ( 'NONE',  ( 0.000000000000000000, 0.000000000000000000, 1.000000000000000000 ) ) ;
#5080 = CARTESIAN_POINT ( 'NONE',  ( -4.458734125000000326, -25.00000000136559564, -1.846868145590735644 ) ) ;
#5081 = DIRECTION ( 'NONE',  ( 0.000000000000000000, 0.000000000000000000, 1.000000000000000000 ) ) ;
#5082 = CIRCLE ( 'NONE', #8970, 2.649999999999992806 ) ;
#5083 = VERTEX_POINT ( 'NONE', #3831 ) ;
#5084 = CARTESIAN_POINT ( 'NONE',  ( 3.455068668934414777, -2.624017327439094327, -3.316620875263732504 ) ) ;
#5085 = PRODUCT_DEFINITION_FORMATION_WITH_SPECIFIED_SOURCE ( 'ANY', '', #9518, .NOT_KNOWN. ) ;
#5086 = VECTOR ( 'NONE', #13815, 1000.000000000000114 ) ;
#5087 = CARTESIAN_POINT ( 'NONE',  ( 2.623433461001182909, -7.604994000793865006, -7.633824513837115688 ) ) ;
#5088 = CARTESIAN_POINT ( 'NONE',  ( 2.131511515620586383, 3.916244202832140253, -1.187499998634405918 ) ) ;
#5089 = DIRECTION ( 'NONE',  ( 0.000000000000000000, 1.000000000000000000, 0.000000000000000000 ) ) ;
#5090 = CARTESIAN_POINT ( 'NONE',  ( 5.000000000000000888, -30.93750000000000355, -2.071067811865475505 ) ) ;
#5091 = DIRECTION ( 'NONE',  ( 0.000000000000000000, 1.000000000000000000, 0.000000000000000000 ) ) ;
#5092 = CIRCLE ( 'NONE', #14131, 30.00000000000000711 ) ;
#5093 = CARTESIAN_POINT ( 'NONE',  ( -17.99999999999979394, -11.00000000000000178, 1.499999999999999112 ) ) ;
#5094 = CARTESIAN_POINT ( 'NONE',  ( 3.535533905932736864, -27.25000000273118772, 3.535533905932738641 ) ) ;
#5095 = CARTESIAN_POINT ( 'NONE',  ( -86.33974596215563224, -97.11324865405184426, 17.50000000000000000 ) ) ;
#5096 = CARTESIAN_POINT ( 'NONE',  ( 4.458734124999999437, -31.43750000136559564, 0.000000000000000000 ) ) ;
#5097 = EDGE_CURVE ( 'NONE', #6462, #11470, #13678, .T. ) ;
#5098 = DIRECTION ( 'NONE',  ( -0.000000000000000000, -1.000000000000000000, -0.000000000000000000 ) ) ;
#5099 = ORIENTED_EDGE ( 'NONE', *, *, #9786, .F. ) ;
#5100 = VERTEX_POINT ( 'NONE', #7646 ) ;
#5101 =( NAMED_UNIT ( * ) SI_UNIT ( $, .STERADIAN. ) SOLID_ANGLE_UNIT ( ) );
#5102 = ORIENTED_EDGE ( 'NONE', *, *, #9405, .F. ) ;
#5103 = CARTESIAN_POINT ( 'NONE',  ( 10.17949192431125915, 0.000000000000000000, -57.63139720814413636 ) ) ;
#5104 = ORIENTED_EDGE ( 'NONE', *, *, #2974, .F. ) ;
#5105 = LINE ( 'NONE', #3806, #15148 ) ;
#5106 = VECTOR ( 'NONE', #2899, 1000.000000000000000 ) ;
#5107 = AXIS2_PLACEMENT_3D ( 'NONE', #10299, #2841, #9003 ) ;
#5108 = CARTESIAN_POINT ( 'NONE',  ( -3.152801135295367096, -31.31250000136559564, -3.152801135295367541 ) ) ;
#5109 = VECTOR ( 'NONE', #13686, 1000.000000000000000 ) ;
#5110 = SHAPE_DEFINITION_REPRESENTATION ( #12976, #1906 ) ;
#5111 = CARTESIAN_POINT ( 'NONE',  ( 2.131511515620586383, 3.916244202832140253, -5.437499998634406140 ) ) ;
#5112 = FACE_OUTER_BOUND ( 'NONE', #3995, .T. ) ;
#5113 = CONICAL_SURFACE ( 'NONE', #6670, 7.500000000000001776, 0.8594454914424796144 ) ;
#5114 = EDGE_CURVE ( 'NONE', #12637, #6791, #12545, .T. ) ;
#5115 = DIRECTION ( 'NONE',  ( 0.8660254037844384856, -0.000000000000000000, 0.5000000000000004441 ) ) ;
#5117 = EDGE_CURVE ( 'NONE', #6271, #15920, #11582, .T. ) ;
#5116 = ORIENTED_EDGE ( 'NONE', *, *, #15078, .T. ) ;
#5118 = CARTESIAN_POINT ( 'NONE',  ( -7.500000000000000000, -4.330127018922196314, -7.422398894150035176 ) ) ;
#5119 = AXIS2_PLACEMENT_3D ( 'NONE', #12872, #11585, #15242 ) ;
#5120 = FILL_AREA_STYLE_COLOUR ( '', #6856 ) ;
#5121 = EDGE_LOOP ( 'NONE', ( #9152, #2682, #10393, #11784, #8317, #10873, #3383 ) ) ;
#5122 = CARTESIAN_POINT ( 'NONE',  ( 35.00000000000000000, 40.00000000000000000, 2.649999999999992806 ) ) ;
#5123 = DIRECTION ( 'NONE',  ( 1.000000000000000000, 0.000000000000000000, 0.000000000000000000 ) ) ;
#5124 = CIRCLE ( 'NONE', #1502, 2.000000000000001776 ) ;
#5125 = ORIENTED_EDGE ( 'NONE', *, *, #3128, .T. ) ;
#5126 = CONTEXT_DEPENDENT_SHAPE_REPRESENTATION ( #7767, #9970 ) ;
#5127 = CARTESIAN_POINT ( 'NONE',  ( 3.753672977998667726, 3.033343224707664820, -6.499999998634408804 ) ) ;
#5128 = DIRECTION ( 'NONE',  ( -0.000000000000000000, -0.000000000000000000, -1.000000000000000000 ) ) ;
#5129 = AXIS2_PLACEMENT_3D ( 'NONE', #7483, #9975, #3834 ) ;
#5130 = VECTOR ( 'NONE', #5585, 1000.000000000000000 ) ;
#5131 = LINE ( 'NONE', #367, #8250 ) ;
#5132 = LINE ( 'NONE', #12384, #14645 ) ;
#5133 = UNCERTAINTY_MEASURE_WITH_UNIT (LENGTH_MEASURE( 1.000000000000000082E-05 ), #12689, 'distance_accuracy_value', 'NONE');
#5134 = CARTESIAN_POINT ( 'NONE',  ( -35.00000000000000000, 50.00000000000000000, 0.000000000000000000 ) ) ;
#5135 = AXIS2_PLACEMENT_3D ( 'NONE', #9093, #15064, #12867 ) ;
#5136 = CARTESIAN_POINT ( 'NONE',  ( -4.795541693661363958, -1.415196051561583790, -5.374999997268817609 ) ) ;
#5137 = LINE ( 'NONE', #5048, #15336 ) ;
#5138 = EDGE_CURVE ( 'NONE', #13545, #15626, #2997, .T. ) ;
#5139 = CARTESIAN_POINT ( 'NONE',  ( -3.912039780753109763, 2.444181052284501110, -0.2789798816695437944 ) ) ;
#5140 = LINE ( 'NONE', #14007, #1939 ) ;
#5141 = EDGE_CURVE ( 'NONE', #6035, #9656, #2928, .T. ) ;
#5142 = ORIENTED_EDGE ( 'NONE', *, *, #3812, .T. ) ;
#5143 = CARTESIAN_POINT ( 'NONE',  ( -5.000000000000004441, -1.011557177027151181E-15, -4.545263047592944083 ) ) ;
#5144 = CARTESIAN_POINT ( 'NONE',  ( -3.033343224707664376, 3.753672977998667726, -6.999999998634408804 ) ) ;
#5145 = CARTESIAN_POINT ( 'NONE',  ( -44.99999999999999289, -25.00000000000000000, -7.500000000000000000 ) ) ;
#5146 = EDGE_LOOP ( 'NONE', ( #3777, #2829 ) ) ;
#5147 = AXIS2_PLACEMENT_3D ( 'NONE', #5421, #498, #10274 ) ;
#5148 = ORIENTED_EDGE ( 'NONE', *, *, #1094, .T. ) ;
#5149 = AXIS2_PLACEMENT_3D ( 'NONE', #9603, #13305, #7201 ) ;
#5150 = ORIENTED_EDGE ( 'NONE', *, *, #15232, .T. ) ;
#5151 = DIRECTION ( 'NONE',  ( 0.000000000000000000, 0.000000000000000000, 1.000000000000000000 ) ) ;
#5152 = CARTESIAN_POINT ( 'NONE',  ( -28.86751345948126257, -35.00000000000000000, -50.00000000000000711 ) ) ;
#5153 = DIRECTION ( 'NONE',  ( 0.000000000000000000, -1.000000000000000000, 0.000000000000000000 ) ) ;
#5154 = CARTESIAN_POINT ( 'NONE',  ( 2.500000000000000000, 0.000000000000000000, 0.000000000000000000 ) ) ;
#5155 = DIRECTION ( 'NONE',  ( 0.000000000000000000, 1.000000000000000000, 0.000000000000000000 ) ) ;
#5156 = LINE ( 'NONE', #11441, #241 ) ;
#5157 = AXIS2_PLACEMENT_3D ( 'NONE', #1390, #14812, #12378 ) ;
#5158 = CARTESIAN_POINT ( 'NONE',  ( -5.381735091635034607, 0.5711823568785950878, -6.562500000000004441 ) ) ;
#5159 = CARTESIAN_POINT ( 'NONE',  ( 2.071067811865451080, -29.81249999999999645, -5.000000000000024869 ) ) ;
#5160 = CARTESIAN_POINT ( 'NONE',  ( 5.000000000000000000, -29.06250000000000000, 2.071067811865478614 ) ) ;
#5161 = CARTESIAN_POINT ( 'NONE',  ( -1.846868145590734756, -26.12500000136559564, -4.458734125000000326 ) ) ;
#5162 = EDGE_CURVE ( 'NONE', #5346, #7134, #7418, .T. ) ;
#5163 = CARTESIAN_POINT ( 'NONE',  ( 4.276409079477644148, 1.261996585732577891, -5.562499998634406140 ) ) ;
#5164 = EDGE_LOOP ( 'NONE', ( #12135, #5201, #5523, #5871 ) ) ;
#5165 = CARTESIAN_POINT ( 'NONE',  ( -1.154700538379261232, -20.00000000000000000, 34.00000000000000000 ) ) ;
#5166 = ORIENTED_EDGE ( 'NONE', *, *, #6898, .F. ) ;
#5167 = VERTEX_POINT ( 'NONE', #11497 ) ;
#5168 = CARTESIAN_POINT ( 'NONE',  ( -3.152801135295367985, -23.81250000136559564, 3.152801135295367096 ) ) ;
#5169 = DIRECTION ( 'NONE',  ( 0.000000000000000000, -1.000000000000000000, 0.000000000000000000 ) ) ;
#5170 = ORIENTED_EDGE ( 'NONE', *, *, #10229, .T. ) ;
#5171 = CARTESIAN_POINT ( 'NONE',  ( -19.99999999999956657, -13.00000000000000178, 8.786575603324269439E-13 ) ) ;
#5172 = DIRECTION ( 'NONE',  ( 0.000000000000000000, 0.000000000000000000, 1.000000000000000000 ) ) ;
#5173 = CARTESIAN_POINT ( 'NONE',  ( -2.131511515620587272, -3.916244202832140253, -0.6874999986344054737 ) ) ;
#5174 = CARTESIAN_POINT ( 'NONE',  ( 1.620853800412707768, 4.162292401171781897, -0.3789984458506779896 ) ) ;
#5175 = CARTESIAN_POINT ( 'NONE',  ( -9.184850993605147944E-16, -31.25000000000000000, 5.000000000000000000 ) ) ;
#5176 = CARTESIAN_POINT ( 'NONE',  ( -4.000000000000000000, -2.309401076758515803, -0.4999999999999995559 ) ) ;
#5177 = PLANE ( 'NONE',  #8760 ) ;
#5178 = CARTESIAN_POINT ( 'NONE',  ( 2.071067811865475505, -28.93750000273119483, -5.000000000000000888 ) ) ;
#5179 = EDGE_CURVE ( 'NONE', #10281, #2882, #11535, .T. ) ;
#5180 = CARTESIAN_POINT ( 'NONE',  ( 4.896370289181586344, 0.000000000000000000, 48.48076211353308906 ) ) ;
#5181 = CARTESIAN_POINT ( 'NONE',  ( 5.000000000000000000, -24.12500000273118772, 0.000000000000000000 ) ) ;
#5182 = SURFACE_STYLE_USAGE ( .BOTH. , #15042 ) ;
#5183 = ORIENTED_EDGE ( 'NONE', *, *, #2547, .F. ) ;
#5184 = ORIENTED_EDGE ( 'NONE', *, *, #10490, .F. ) ;
#5185 = ORIENTED_EDGE ( 'NONE', *, *, #12542, .T. ) ;
#5186 = CARTESIAN_POINT ( 'NONE',  ( 12.67949192431120586, 0.000000000000000000, 61.96152422706632024 ) ) ;
#5187 = ORIENTED_EDGE ( 'NONE', *, *, #6405, .T. ) ;
#5188 = CARTESIAN_POINT ( 'NONE',  ( 3.061616997868383141E-16, -24.87500000273118417, -5.000000000000000000 ) ) ;
#5189 = EDGE_CURVE ( 'NONE', #9703, #1037, #12700, .T. ) ;
#5190 = CARTESIAN_POINT ( 'NONE',  ( 7.914973979435151463, 3.817460047930444134, -7.907502498112419786 ) ) ;
#5191 = CARTESIAN_POINT ( 'NONE',  ( 3.152801135295367541, -30.56250000136559564, -3.152801135295367541 ) ) ;
#5192 =( NAMED_UNIT ( * ) SI_UNIT ( $, .STERADIAN. ) SOLID_ANGLE_UNIT ( ) );
#5193 = CARTESIAN_POINT ( 'NONE',  ( 1.261996585732578113, -4.276409079477644148, -5.812499998634406140 ) ) ;
#5194 = DIRECTION ( 'NONE',  ( 0.000000000000000000, 0.000000000000000000, 1.000000000000000000 ) ) ;
#5195 = DIRECTION ( 'NONE',  ( 0.000000000000000000, 0.000000000000000000, -1.000000000000000000 ) ) ;
#5196 = ORIENTED_EDGE ( 'NONE', *, *, #15736, .T. ) ;
#5197 = DIRECTION ( 'NONE',  ( -0.9396926207859138680, 0.000000000000000000, -0.3420201433256536139 ) ) ;
#5198 = FILL_AREA_STYLE_COLOUR ( '', #5560 ) ;
#5199 = ORIENTED_EDGE ( 'NONE', *, *, #12225, .F. ) ;
#5200 = CARTESIAN_POINT ( 'NONE',  ( 4.391654775818395251, -2.390265326283149694, -7.125000000000002665 ) ) ;
#5201 = ORIENTED_EDGE ( 'NONE', *, *, #14506, .F. ) ;
#5202 = CARTESIAN_POINT ( 'NONE',  ( -0.5093500532425060401, -4.799145180956616130, -6.874999998634407916 ) ) ;
#5203 = EDGE_CURVE ( 'NONE', #11426, #7997, #13585, .T. ) ;
#5204 = EDGE_CURVE ( 'NONE', #1816, #4597, #6018, .T. ) ;
#5205 = FACE_OUTER_BOUND ( 'NONE', #6559, .T. ) ;
#5206 = CARTESIAN_POINT ( 'NONE',  ( 2.071067811865462183, -21.31250000273118772, 5.000000000000013323 ) ) ;
#5207 = DIRECTION ( 'NONE',  ( 0.000000000000000000, -0.000000000000000000, 1.000000000000000000 ) ) ;
#5208 = CARTESIAN_POINT ( 'NONE',  ( 2.390265326283148806, 4.391654775818395251, -5.749999997268814944 ) ) ;
#5209 = CARTESIAN_POINT ( 'NONE',  ( -5.000000000000000000, -23.50000000000000000, -6.123233995736766282E-16 ) ) ;
#5210 = CARTESIAN_POINT ( 'NONE',  ( -1.502104865711912707, 4.262924311968062874, -0.3382386524005038808 ) ) ;
#5211 = CARTESIAN_POINT ( 'NONE',  ( 4.458734124999997661, -21.75000000136559208, 1.846868145590737864 ) ) ;
#5212 = VERTEX_POINT ( 'NONE', #5451 ) ;
#5213 = DIRECTION ( 'NONE',  ( 0.000000000000000000, 0.000000000000000000, 1.000000000000000000 ) ) ;
#5214 = CARTESIAN_POINT ( 'NONE',  ( 1.261996585732578113, -4.276409079477644148, -7.562499998634407916 ) ) ;
#5215 = LINE ( 'NONE', #12555, #7911 ) ;
#5216 = ORIENTED_EDGE ( 'NONE', *, *, #734, .F. ) ;
#5217 = ORIENTED_EDGE ( 'NONE', *, *, #5114, .F. ) ;
#5218 =( BOUNDED_CURVE ( )  B_SPLINE_CURVE ( 3, ( #11904, #13121, #9797, #9500 ),
 .UNSPECIFIED., .F., .F. ) 
 B_SPLINE_CURVE_WITH_KNOTS ( ( 4, 4 ),
 ( 1.570796326794896780, 3.141592653589793116 ),
 .UNSPECIFIED. ) 
 CURVE ( )  GEOMETRIC_REPRESENTATION_ITEM ( )  RATIONAL_B_SPLINE_CURVE ( ( 1.000000000000000000, 0.8047378541243650485, 0.8047378541243650485, 1.000000000000000000 ) ) 
 REPRESENTATION_ITEM ( '' )  );
#5219 = ORIENTED_EDGE ( 'NONE', *, *, #4312, .F. ) ;
#5220 = LINE ( 'NONE', #6519, #15150 ) ;
#5221 = CARTESIAN_POINT ( 'NONE',  ( -55.00000000000000000, -10.00000000000000178, -17.50000000000000000 ) ) ;
#5222 = CARTESIAN_POINT ( 'NONE',  ( -3.535533905932738641, -27.50000000273118772, 3.535533905932737309 ) ) ;
#5223 = EDGE_CURVE ( 'NONE', #14394, #2454, #6907, .T. ) ;
#5224 = CARTESIAN_POINT ( 'NONE',  ( -6.602753909532900423, -5.319290460493544259, -7.792447862505331280 ) ) ;
#5225 = CARTESIAN_POINT ( 'NONE',  ( -0.3306966981844624009, -8.469326210127480437, -7.349897473154090477 ) ) ;
#5226 = LINE ( 'NONE', #15087, #994 ) ;
#5227 = AXIS2_PLACEMENT_3D ( 'NONE', #6476, #7697, #10426 ) ;
#5228 = CARTESIAN_POINT ( 'NONE',  ( -2.390265326283148806, -4.391654775818394363, -3.375000000000003109 ) ) ;
#5229 = DIRECTION ( 'NONE',  ( -0.4999999999999976685, -0.8660254037844399289, 0.000000000000000000 ) ) ;
#5230 = LINE ( 'NONE', #15089, #6926 ) ;
#5231 = CARTESIAN_POINT ( 'NONE',  ( 3.152801135295366208, -22.56250000136559564, 3.152801135295367985 ) ) ;
#5232 = CARTESIAN_POINT ( 'NONE',  ( -0.5093500532425060401, -4.799145180956616130, -5.874999998634406140 ) ) ;
#5233 = EDGE_LOOP ( 'NONE', ( #15663, #2764 ) ) ;
#5234 = CARTESIAN_POINT ( 'NONE',  ( 5.000000000000000888, 0.000000000000000000, -25.03750572909317285 ) ) ;
#5235 = ORIENTED_EDGE ( 'NONE', *, *, #14818, .T. ) ;
#5236 = ORIENTED_EDGE ( 'NONE', *, *, #3940, .T. ) ;
#5237 = CARTESIAN_POINT ( 'NONE',  ( -1.846868145590737420, -30.00000000136559564, 4.458734124999999437 ) ) ;
#5238 = CARTESIAN_POINT ( 'NONE',  ( -91.33974596215560382, -110.0591436588189396, 7.500000000000001776 ) ) ;
#5239 = VERTEX_POINT ( 'NONE', #9404 ) ;
#5240 = VECTOR ( 'NONE', #7286, 1000.000000000000000 ) ;
#5241 = CARTESIAN_POINT ( 'NONE',  ( 2.712762565639649015, -3.052587955997662306, -3.430618716626630871 ) ) ;
#5242 = EDGE_CURVE ( 'NONE', #794, #14464, #15480, .T. ) ;
#5243 = ADVANCED_FACE ( 'NONE', ( #4227 ), #9170, .T. ) ;
#5244 = EDGE_CURVE ( 'NONE', #6090, #15006, #5686, .T. ) ;
#5245 = ADVANCED_FACE ( 'NONE', ( #11654 ), #12563, .F. ) ;
#5246 = CARTESIAN_POINT ( 'NONE',  ( 7.922281120364393914, -4.573931137438281169, -8.047472243342932430 ) ) ;
#5247 = CARTESIAN_POINT ( 'NONE',  ( 4.276409079477644148, 1.261996585732577891, -2.312499998634407028 ) ) ;
#5248 = CARTESIAN_POINT ( 'NONE',  ( 0.000000000000000000, -20.00000000000000000, 0.000000000000000000 ) ) ;
#5249 = CARTESIAN_POINT ( 'NONE',  ( 3.535533905932738197, -30.87500000000000000, -3.535533905932738197 ) ) ;
#5250 = CARTESIAN_POINT ( 'NONE',  ( -3.349226789952655547, -2.685125164760744809, -0.2236248678334863682 ) ) ;
#5251 = DIRECTION ( 'NONE',  ( -0.000000000000000000, -1.000000000000000000, -0.000000000000000000 ) ) ;
#5252 = CARTESIAN_POINT ( 'NONE',  ( 5.000000000000000888, -23.06250000273118417, -2.071067811865475505 ) ) ;
#5253 = DIRECTION ( 'NONE',  ( -0.000000000000000000, -1.000000000000000000, -0.000000000000000000 ) ) ;
#5254 = CARTESIAN_POINT ( 'NONE',  ( -4.458734124999999437, -30.93750000136559564, -5.460374474430324690E-16 ) ) ;
#5255 =( LENGTH_UNIT ( ) NAMED_UNIT ( * ) SI_UNIT ( .MILLI., .METRE. ) );
#5256 = ORIENTED_EDGE ( 'NONE', *, *, #3512, .T. ) ;
#5257 = ORIENTED_EDGE ( 'NONE', *, *, #6740, .T. ) ;
#5258 = ORIENTED_EDGE ( 'NONE', *, *, #4143, .T. ) ;
#5259 = CARTESIAN_POINT ( 'NONE',  ( -44.40593521050208636, -4.342938577512204468, 20.10634714468941908 ) ) ;
#5260 = ORIENTED_EDGE ( 'NONE', *, *, #8366, .F. ) ;
#5261 = CARTESIAN_POINT ( 'NONE',  ( 0.000000000000000000, -13.00000000000000178, 0.000000000000000000 ) ) ;
#5262 = EDGE_CURVE ( 'NONE', #5482, #5812, #10458, .T. ) ;
#5263 =( REPRESENTATION_RELATIONSHIP ('NONE','NONE', #4176, #1906 ) REPRESENTATION_RELATIONSHIP_WITH_TRANSFORMATION ( #1315 )SHAPE_REPRESENTATION_RELATIONSHIP( ) );
#5264 = CARTESIAN_POINT ( 'NONE',  ( 5.000000000000091482, 0.7223674278660682235, -1.896799362785968945 ) ) ;
#5265 = DIRECTION ( 'NONE',  ( 0.000000000000000000, 0.000000000000000000, 1.000000000000000000 ) ) ;
#5266 = CARTESIAN_POINT ( 'NONE',  ( -5.000000000000004441, -1.011557177027151181E-15, -5.545263047592944972 ) ) ;
#5267 = PRODUCT_CONTEXT ( 'NONE', #8162, 'mechanical' ) ;
#5268 = CARTESIAN_POINT ( 'NONE',  ( -1.261996585732579224, 4.276409079477648589, -5.312499998634406140 ) ) ;
#5269 = DIRECTION ( 'NONE',  ( 1.000000000000000000, 3.851859888774473808E-30, -1.387778780781445676E-15 ) ) ;
#5270 = ORIENTED_EDGE ( 'NONE', *, *, #6700, .F. ) ;
#5271 = CARTESIAN_POINT ( 'NONE',  ( 4.882921219558935988, -4.732646668675131174, -48.48447359618705121 ) ) ;
#5272 =( LENGTH_UNIT ( ) NAMED_UNIT ( * ) SI_UNIT ( .MILLI., .METRE. ) );
#5273 = ORIENTED_EDGE ( 'NONE', *, *, #2, .F. ) ;
#5274 = CARTESIAN_POINT ( 'NONE',  ( -5.000000000000004441, -7.530481206757679743E-15, -1.545263047592943861 ) ) ;
#5275 = DIRECTION ( 'NONE',  ( -8.673617379884037444E-16, 0.000000000000000000, -1.000000000000000000 ) ) ;
#5276 = AXIS2_PLACEMENT_3D ( 'NONE', #11192, #12474, #7330 ) ;
#5277 = ORIENTED_EDGE ( 'NONE', *, *, #7751, .F. ) ;
#5278 = ITEM_DEFINED_TRANSFORMATION ( 'NONE', 'NONE', #7101,  #3223 ) ;
#5279 = CARTESIAN_POINT ( 'NONE',  ( 0.5093500532425063732, 4.799145180956616130, -6.374999998634408804 ) ) ;
#5280 = CIRCLE ( 'NONE', #2421, 0.2500000000000002220 ) ;
#5281 = DIRECTION ( 'NONE',  ( 0.000000000000000000, 1.000000000000000000, 0.000000000000000000 ) ) ;
#5282 = DIRECTION ( 'NONE',  ( -0.000000000000000000, -1.000000000000000000, -0.000000000000000000 ) ) ;
#5283 = DIRECTION ( 'NONE',  ( -0.000000000000000000, -1.000000000000000000, -0.000000000000000000 ) ) ;
#5284 = VECTOR ( 'NONE', #9338, 1000.000000000000000 ) ;
#5285 = AXIS2_PLACEMENT_3D ( 'NONE', #7288, #3185, #4776 ) ;
#5286 = CARTESIAN_POINT ( 'NONE',  ( 3.401574460001763001, -4.209348295687703967, -4.062499997268816720 ) ) ;
#5287 = CARTESIAN_POINT ( 'NONE',  ( 0.6666666666666658525, -4.233901974057276085, -3.300726591567086476 ) ) ;
#5288 = CARTESIAN_POINT ( 'NONE',  ( -4.671041856245029322, -9.682850088987660890E-14, -0.2303389720127052009 ) ) ;
#5289 = PLANE ( 'NONE',  #6859 ) ;
#5290 = VERTEX_POINT ( 'NONE', #4317 ) ;
#5291 = AXIS2_PLACEMENT_3D ( 'NONE', #4225, #6747, #9253 ) ;
#5292 = DIRECTION ( 'NONE',  ( -0.000000000000000000, -1.000000000000000000, -0.000000000000000000 ) ) ;
#5293 = CARTESIAN_POINT ( 'NONE',  ( 7.500000000000001776, 3.608439182435154269, -7.298562697733103732 ) ) ;
#5294 = DIRECTION ( 'NONE',  ( 0.000000000000000000, 0.000000000000000000, 1.000000000000000000 ) ) ;
#5295 = EDGE_CURVE ( 'NONE', #7703, #2885, #3796, .T. ) ;
#5296 = EDGE_LOOP ( 'NONE', ( #5166, #15581, #985, #9163 ) ) ;
#5297 = ORIENTED_EDGE ( 'NONE', *, *, #1180, .F. ) ;
#5298 = EDGE_CURVE ( 'NONE', #13118, #3154, #12614, .T. ) ;
#5299 = ORIENTED_EDGE ( 'NONE', *, *, #6961, .F. ) ;
#5300 = CARTESIAN_POINT ( 'NONE',  ( -5.000000000000004441, -7.530481206757679743E-15, -0.5452630475929430842 ) ) ;
#5301 = FACE_BOUND ( 'NONE', #6982, .T. ) ;
#5302 = AXIS2_PLACEMENT_3D ( 'NONE', #13899, #10357, #10279 ) ;
#5303 = CARTESIAN_POINT ( 'NONE',  ( 6.123233995736766282E-16, -13.00000000000000178, -5.000000000000000000 ) ) ;
#5304 = AXIS2_PLACEMENT_3D ( 'NONE', #531, #15233, #8044 ) ;
#5305 = DIRECTION ( 'NONE',  ( -1.000000000000000000, 0.000000000000000000, 0.000000000000000000 ) ) ;
#5306 = LINE ( 'NONE', #11287, #1092 ) ;
#5307 = DIRECTION ( 'NONE',  ( 0.000000000000000000, 0.000000000000000000, 1.000000000000000000 ) ) ;
#5308 = CARTESIAN_POINT ( 'NONE',  ( 3.401574460001763001, -4.209348295687703967, -7.187500000000003553 ) ) ;
#5309 = CARTESIAN_POINT ( 'NONE',  ( 4.795541693661363958, 1.415196051561583790, -3.000000000000002665 ) ) ;
#5310 = CARTESIAN_POINT ( 'NONE',  ( -2.756197834950067094, -3.027510591568735254, -3.223146290109809797 ) ) ;
#5311 = CARTESIAN_POINT ( 'NONE',  ( 4.458734124999999437, -22.43750000136559564, 0.000000000000000000 ) ) ;
#5312 =( BOUNDED_CURVE ( )  B_SPLINE_CURVE ( 3, ( #2060, #6691, #15496, #12885 ),
 .UNSPECIFIED., .F., .F. ) 
 B_SPLINE_CURVE_WITH_KNOTS ( ( 4, 4 ),
 ( 3.141592653589793116, 4.712388980384689674 ),
 .UNSPECIFIED. ) 
 CURVE ( )  GEOMETRIC_REPRESENTATION_ITEM ( )  RATIONAL_B_SPLINE_CURVE ( ( 1.000000000000000000, 0.8047378541243649375, 0.8047378541243649375, 1.000000000000000000 ) ) 
 REPRESENTATION_ITEM ( '' )  );
#5313 = CARTESIAN_POINT ( 'NONE',  ( -3.916244202832140253, 2.131511515620587272, -8.187499998634407916 ) ) ;
#5314 = EDGE_LOOP ( 'NONE', ( #1230, #2678, #638, #14337 ) ) ;
#5315 = CIRCLE ( 'NONE', #11495, 25.00000000000000000 ) ;
#5316 = CARTESIAN_POINT ( 'NONE',  ( 1.411581201560190495E-15, 4.862606272033091592, -3.745885042887436622 ) ) ;
#5317 = ADVANCED_FACE ( 'NONE', ( #4631 ), #13657, .F. ) ;
#5318 = ORIENTED_EDGE ( 'NONE', *, *, #6737, .F. ) ;
#5319 = ORIENTED_EDGE ( 'NONE', *, *, #8718, .F. ) ;
#5320 = EDGE_CURVE ( 'NONE', #9210, #12212, #6137, .T. ) ;
#5321 = VECTOR ( 'NONE', #14541, 999.9999999999998863 ) ;
#5322 = AXIS2_PLACEMENT_3D ( 'NONE', #12904, #5719, #5487 ) ;
#5323 = ORIENTED_EDGE ( 'NONE', *, *, #3902, .T. ) ;
#5324 = CARTESIAN_POINT ( 'NONE',  ( -4.458734124999999437, -31.18750000136559564, -5.460374474430324690E-16 ) ) ;
#5325 = CARTESIAN_POINT ( 'NONE',  ( 3.061616997868383141E-16, -21.87500000273118772, -5.000000000000000000 ) ) ;
#5326 = ORIENTED_EDGE ( 'NONE', *, *, #6221, .F. ) ;
#5327 = CARTESIAN_POINT ( 'NONE',  ( 3.522875095019493141, -2.820352903225631369, -3.598441714920572299 ) ) ;
#5328 = VECTOR ( 'NONE', #14495, 1000.000000000000000 ) ;
#5329 = DIRECTION ( 'NONE',  ( -0.5000000000000016653, 0.8660254037844378194, 0.000000000000000000 ) ) ;
#5330 = CARTESIAN_POINT ( 'NONE',  ( 3.916244202832140253, -2.131511515620588160, -0.4374999986344086933 ) ) ;
#5331 = CARTESIAN_POINT ( 'NONE',  ( 3.175402709531165435, 3.141463792224340690, -0.3789984458506759912 ) ) ;
#5332 = VECTOR ( 'NONE', #11612, 1000.000000000000000 ) ;
#5333 = CARTESIAN_POINT ( 'NONE',  ( 3.535533905932736864, -29.12500000000000000, 3.535533905932738641 ) ) ;
#5334 = CARTESIAN_POINT ( 'NONE',  ( -3.916244202832140253, 2.131511515620587272, -1.937499998634406584 ) ) ;
#5335 = CARTESIAN_POINT ( 'NONE',  ( -0.3461262719736137305, 4.658553426539289610, -3.671615880910373608 ) ) ;
#5336 = DIRECTION ( 'NONE',  ( 1.000000000000000000, 0.000000000000000000, -1.239088197126290570E-16 ) ) ;
#5337 = CARTESIAN_POINT ( 'NONE',  ( 3.535533905932738197, -23.00000000273118772, -3.535533905932738197 ) ) ;
#5338 = CARTESIAN_POINT ( 'NONE',  ( 0.000000000000000000, 2.000000000000000000, 0.000000000000000000 ) ) ;
#5339 = CARTESIAN_POINT ( 'NONE',  ( 3.152801135295367541, -25.31250000136559564, -3.152801135295367541 ) ) ;
#5340 = EDGE_CURVE ( 'NONE', #715, #2379, #5092, .T. ) ;
#5341 = CARTESIAN_POINT ( 'NONE',  ( -21.01110699893060030, 2.000000000000000000, 39.04230484541323420 ) ) ;
#5342 = ORIENTED_EDGE ( 'NONE', *, *, #9521, .F. ) ;
#5343 = CIRCLE ( 'NONE', #14370, 10.00000000000000533 ) ;
#5344 = ORIENTED_EDGE ( 'NONE', *, *, #13132, .F. ) ;
#5345 = ADVANCED_FACE ( 'NONE', ( #15420 ), #7694, .F. ) ;
#5346 = VERTEX_POINT ( 'NONE', #6769 ) ;
#5347 = CARTESIAN_POINT ( 'NONE',  ( -44.01413460128225807, -3.061199086701614114, 21.49255004891554677 ) ) ;
#5348 = PRODUCT_DEFINITION_FORMATION_WITH_SPECIFIED_SOURCE ( 'ANY', '', #9629, .NOT_KNOWN. ) ;
#5349 = VERTEX_POINT ( 'NONE', #7010 ) ;
#5350 = CARTESIAN_POINT ( 'NONE',  ( 23.49999999999956657, -8.782289339527253835E-13, 0.000000000000000000 ) ) ;
#5351 = VECTOR ( 'NONE', #15085, 1000.000000000000000 ) ;
#5352 = CARTESIAN_POINT ( 'NONE',  ( -5.000000000000004441, -7.530481206757679743E-15, -1.420263044861758361 ) ) ;
#5353 = CARTESIAN_POINT ( 'NONE',  ( -1.846868145590734756, -30.37500000136559564, -4.458734125000000326 ) ) ;
#5354 = CARTESIAN_POINT ( 'NONE',  ( 0.5711823568785988625, 5.381735091635026613, -0.6874999972688190519 ) ) ;
#5355 = ITEM_DEFINED_TRANSFORMATION ( 'NONE', 'NONE', #7874,  #3223 ) ;
#5356 = CARTESIAN_POINT ( 'NONE',  ( -1.415196051561583790, 4.795541693661363958, -7.624999997268816720 ) ) ;
#5357 = AXIS2_PLACEMENT_3D ( 'NONE', #15080, #12560, #9110 ) ;
#5358 = DIRECTION ( 'NONE',  ( 0.5000000000000002220, -1.734723475976806503E-15, 0.8660254037844383745 ) ) ;
#5359 = EDGE_CURVE ( 'NONE', #3959, #1601, #9920, .T. ) ;
#5360 = ORIENTED_EDGE ( 'NONE', *, *, #3426, .F. ) ;
#5361 = EDGE_CURVE ( 'NONE', #10378, #8374, #4251, .T. ) ;
#5362 = ORIENTED_EDGE ( 'NONE', *, *, #14391, .T. ) ;
#5363 = CARTESIAN_POINT ( 'NONE',  ( 3.401574460001763445, -4.209348295687703079, -7.187500000000003553 ) ) ;
#5364 = AXIS2_PLACEMENT_3D ( 'NONE', #1240, #3745, #2689 ) ;
#5365 = CARTESIAN_POINT ( 'NONE',  ( -1.846868145590734756, -31.12500000136559564, -4.458734125000000326 ) ) ;
#5366 = EDGE_LOOP ( 'NONE', ( #14016, #14928, #1525, #9554 ) ) ;
#5367 = CARTESIAN_POINT ( 'NONE',  ( -3.916244202832140253, 2.131511515620587272, -7.187499998634407916 ) ) ;
#5368 = PRESENTATION_STYLE_ASSIGNMENT (( #14087 ) ) ;
#5369 = CARTESIAN_POINT ( 'NONE',  ( 3.401574460001763445, -4.209348295687703079, -5.062499997268816720 ) ) ;
#5370 = CIRCLE ( 'NONE', #1754, 32.00000000000000711 ) ;
#5371 = CARTESIAN_POINT ( 'NONE',  ( -21.01110699893041556, 2.000000000000000000, -36.39230484541334221 ) ) ;
#5372 = CARTESIAN_POINT ( 'NONE',  ( 4.209348295687701302, 3.401574460001765665, -2.812499997268815388 ) ) ;
#5373 = DIRECTION ( 'NONE',  ( 0.000000000000000000, 0.000000000000000000, -1.000000000000000000 ) ) ;
#5374 = DIRECTION ( 'NONE',  ( -0.000000000000000000, -1.000000000000000000, -0.000000000000000000 ) ) ;
#5375 = CARTESIAN_POINT ( 'NONE',  ( -3.152801135295367096, -23.31250000136559564, -3.152801135295367541 ) ) ;
#5376 = VERTEX_POINT ( 'NONE', #630 ) ;
#5377 = FACE_OUTER_BOUND ( 'NONE', #11720, .T. ) ;
#5378 = CARTESIAN_POINT ( 'NONE',  ( -4.276409079477644148, -1.261996585732578335, -7.812499998634407916 ) ) ;
#5379 = ADVANCED_FACE ( 'NONE', ( #14117 ), #10484, .F. ) ;
#5380 = AXIS2_PLACEMENT_3D ( 'NONE', #6254, #6496, #8681 ) ;
#5381 = DIRECTION ( 'NONE',  ( 0.000000000000000000, 0.000000000000000000, 1.000000000000000000 ) ) ;
#5382 = ORIENTED_EDGE ( 'NONE', *, *, #4019, .F. ) ;
#5383 = CARTESIAN_POINT ( 'NONE',  ( -4.000000000000000000, 2.471528634177585282, -3.686887442155186712 ) ) ;
#5384 = ORIENTED_EDGE ( 'NONE', *, *, #15833, .T. ) ;
#5385 = ORIENTED_EDGE ( 'NONE', *, *, #11619, .F. ) ;
#5386 = LINE ( 'NONE', #7749, #1737 ) ;
#5387 = DIRECTION ( 'NONE',  ( 0.000000000000000000, 0.000000000000000000, 1.000000000000000000 ) ) ;
#5388 = CIRCLE ( 'NONE', #6419, 32.00000000000000711 ) ;
#5389 = CYLINDRICAL_SURFACE ( 'NONE', #9665, 5.000000000000000000 ) ;
#5390 = AXIS2_PLACEMENT_3D ( 'NONE', #4806, #6188, #3300 ) ;
#5391 = EDGE_CURVE ( 'NONE', #10154, #59, #1478, .T. ) ;
#5392 = DIRECTION ( 'NONE',  ( 0.000000000000000000, 0.000000000000000000, 1.000000000000000000 ) ) ;
#5393 = DIRECTION ( 'NONE',  ( -1.000000000000000000, 0.000000000000000000, -0.000000000000000000 ) ) ;
#5394 = DIRECTION ( 'NONE',  ( -0.000000000000000000, 1.000000000000000000, -0.000000000000000000 ) ) ;
#5395 = CARTESIAN_POINT ( 'NONE',  ( 5.381735091635035495, -0.5711823568785978633, -6.062500000000000000 ) ) ;
#5396 = DIRECTION ( 'NONE',  ( 0.000000000000000000, 0.000000000000000000, -1.000000000000000000 ) ) ;
#5397 = AXIS2_PLACEMENT_3D ( 'NONE', #11674, #5550, #9116 ) ;
#5398 = FACE_OUTER_BOUND ( 'NONE', #3723, .T. ) ;
#5399 = DIRECTION ( 'NONE',  ( 0.000000000000000000, 0.000000000000000000, 1.000000000000000000 ) ) ;
#5400 = AXIS2_PLACEMENT_3D ( 'NONE', #5720, #4111, #9059 ) ;
#5401 = CARTESIAN_POINT ( 'NONE',  ( -4.276409079477644148, -1.261996585732578335, -8.062499998634407916 ) ) ;
#5402 = VERTEX_POINT ( 'NONE', #5633 ) ;
#5403 = DIRECTION ( 'NONE',  ( -1.000000000000000000, 0.000000000000000000, 1.239088197126290570E-16 ) ) ;
#5404 = EDGE_LOOP ( 'NONE', ( #897, #6728, #8945, #4656 ) ) ;
#5405 = ORIENTED_EDGE ( 'NONE', *, *, #5117, .F. ) ;
#5406 = VERTEX_POINT ( 'NONE', #3124 ) ;
#5407 = CARTESIAN_POINT ( 'NONE',  ( -4.458734125000001214, -31.12500000136559564, 1.846868145590734089 ) ) ;
#5408 = CARTESIAN_POINT ( 'NONE',  ( 0.000000000000000000, -20.00000000000000000, 1.500000000000000000 ) ) ;
#5409 = ORIENTED_EDGE ( 'NONE', *, *, #14328, .F. ) ;
#5410 = CARTESIAN_POINT ( 'NONE',  ( 1.257172072275274388, -3.892973519170983110, -3.433252694550781303 ) ) ;
#5411 = VECTOR ( 'NONE', #3352, 1000.000000000000000 ) ;
#5412 = CARTESIAN_POINT ( 'NONE',  ( 7.915340744419800068, 3.857466640755369713, -7.913699667208869748 ) ) ;
#5413 = EDGE_CURVE ( 'NONE', #15345, #3118, #5551, .T. ) ;
#5414 = CARTESIAN_POINT ( 'NONE',  ( -4.799145180956616130, 0.5093500532425063732, -2.874999998634407472 ) ) ;
#5415 = CARTESIAN_POINT ( 'NONE',  ( 67.49999999999931788, 40.00000000000000000, -2.649999999999971934 ) ) ;
#5416 = EDGE_CURVE ( 'NONE', #5083, #10519, #8981, .T. ) ;
#5417 =( BOUNDED_CURVE ( )  B_SPLINE_CURVE ( 2, ( #14668, #12304, #1241, #6190, #11983, #15886, #13271, #9646, #4960, #46, #8307 ),
 .UNSPECIFIED., .F., .F. ) 
 B_SPLINE_CURVE_WITH_KNOTS ( ( 3, 2, 2, 2, 2, 3 ),
 ( 0.4045872658012772960, 0.4124999999999999778, 0.4249999999999999889, 0.4375000000000000000, 0.4500000000000000111, 0.4545872658012772849 ),
 .UNSPECIFIED. ) 
 CURVE ( )  GEOMETRIC_REPRESENTATION_ITEM ( )  RATIONAL_B_SPLINE_CURVE ( ( 0.9646335149384805963, 0.9518143178943438976, 1.000000000000000000, 0.9238795325112867385, 1.000000000000000000, 0.9238795325112867385, 1.000000000000000000, 0.9238795325112867385, 1.000000000000000000, 0.9720652146169430630, 0.9646335149384808183 ) ) 
 REPRESENTATION_ITEM ( '' )  );
#5418 = CARTESIAN_POINT ( 'NONE',  ( -3.535533905932737309, -25.62500000000000355, -3.535533905932738197 ) ) ;
#5419 = CARTESIAN_POINT ( 'NONE',  ( 1.261996585732578113, -4.276409079477644148, -5.562499998634406140 ) ) ;
#5420 = CARTESIAN_POINT ( 'NONE',  ( -44.21674811821717554, -3.395032785697067901, -20.79966053514407420 ) ) ;
#5421 = CARTESIAN_POINT ( 'NONE',  ( -43.99999999999978684, -9.000000000000001776, -1.500000000000000666 ) ) ;
#5422 = CARTESIAN_POINT ( 'NONE',  ( -2.071067811865478170, -24.43750000273119483, 5.000000000000000000 ) ) ;
#5423 = CARTESIAN_POINT ( 'NONE',  ( -4.209348295687703079, -3.401574460001763445, -3.437500000000003553 ) ) ;
#5424 = CARTESIAN_POINT ( 'NONE',  ( -1.846868145590734756, -28.12500000136559564, -4.458734124999999437 ) ) ;
#5425 = CARTESIAN_POINT ( 'NONE',  ( 7.112481253774558532, -4.553861071371746227, -7.781689322726583313 ) ) ;
#5426 = VERTEX_POINT ( 'NONE', #3199 ) ;
#5427 = ORIENTED_EDGE ( 'NONE', *, *, #3362, .F. ) ;
#5428 = CARTESIAN_POINT ( 'NONE',  ( 4.211140560182196957, -2.431303136016555122, -3.745885042887436622 ) ) ;
#5429 = ORIENTED_EDGE ( 'NONE', *, *, #7499, .F. ) ;
#5430 = CARTESIAN_POINT ( 'NONE',  ( 7.549006887134069643, 4.358421158401189821, -7.700127545397313256 ) ) ;
#5431 = VERTEX_POINT ( 'NONE', #8148 ) ;
#5432 = DIRECTION ( 'NONE',  ( 0.000000000000000000, 0.000000000000000000, -1.000000000000000000 ) ) ;
#5433 = EDGE_CURVE ( 'NONE', #10705, #11234, #13045, .T. ) ;
#5434 = DIRECTION ( 'NONE',  ( 0.000000000000000000, 1.000000000000000000, 0.000000000000000000 ) ) ;
#5435 = EDGE_CURVE ( 'NONE', #1886, #15020, #2066, .T. ) ;
#5436 = FACE_BOUND ( 'NONE', #5146, .T. ) ;
#5437 = LINE ( 'NONE', #6489, #9850 ) ;
#5438 = CONTEXT_DEPENDENT_SHAPE_REPRESENTATION ( #2461, #14161 ) ;
#5439 = FACE_OUTER_BOUND ( 'NONE', #11297, .T. ) ;
#5440 = DIRECTION ( 'NONE',  ( -0.000000000000000000, -1.000000000000000000, -0.000000000000000000 ) ) ;
#5441 = ORIENTED_EDGE ( 'NONE', *, *, #15616, .F. ) ;
#5442 = ORIENTED_EDGE ( 'NONE', *, *, #14990, .F. ) ;
#5443 = FACE_OUTER_BOUND ( 'NONE', #13159, .T. ) ;
#5444 = CARTESIAN_POINT ( 'NONE',  ( -1.846868145590734756, -27.12500000136559564, -4.458734125000000326 ) ) ;
#5445 = ORIENTED_EDGE ( 'NONE', *, *, #9103, .F. ) ;
#5446 = CARTESIAN_POINT ( 'NONE',  ( 5.000000000000002665, 1.275685995473128912E-14, -5.045263047592944083 ) ) ;
#5447 = EDGE_CURVE ( 'NONE', #6256, #14832, #9487, .T. ) ;
#5448 = EDGE_CURVE ( 'NONE', #14100, #9570, #2499, .T. ) ;
#5449 = EDGE_CURVE ( 'NONE', #14394, #11190, #10960, .T. ) ;
#5450 = CARTESIAN_POINT ( 'NONE',  ( -5.000000000000095035, -0.7223674278660573433, -5.396799362785971610 ) ) ;
#5451 = CARTESIAN_POINT ( 'NONE',  ( -24.26932219902319687, 40.00000000000000000, -5.999999999999984901 ) ) ;
#5452 = CARTESIAN_POINT ( 'NONE',  ( 0.5711823568785989735, 5.381735091635026613, -6.687499997268816720 ) ) ;
#5453 = LINE ( 'NONE', #4400, #3871 ) ;
#5454 = CARTESIAN_POINT ( 'NONE',  ( -67.50000000000000000, 50.00000000000000000, -7.070249711157346244E-13 ) ) ;
#5455 = CARTESIAN_POINT ( 'NONE',  ( -4.458734125000000326, -22.12500000136559564, 1.846868145590734089 ) ) ;
#5456 = EDGE_LOOP ( 'NONE', ( #15248, #2749, #9377, #11898 ) ) ;
#5457 = CARTESIAN_POINT ( 'NONE',  ( -90.00000000000000000, -95.00000000000000000, -7.500000000000000000 ) ) ;
#5458 = CARTESIAN_POINT ( 'NONE',  ( -3.916244202832140253, 2.131511515620587272, -6.937499998634407916 ) ) ;
#5459 = DIRECTION ( 'NONE',  ( -0.000000000000000000, 1.000000000000000000, -0.000000000000000000 ) ) ;
#5460 = VERTEX_POINT ( 'NONE', #8383 ) ;
#5461 = CYLINDRICAL_SURFACE ( 'NONE', #15745, 2.499999999999998668 ) ;
#5462 = ORIENTED_EDGE ( 'NONE', *, *, #9108, .T. ) ;
#5463 = ORIENTED_EDGE ( 'NONE', *, *, #9039, .F. ) ;
#5464 = CARTESIAN_POINT ( 'NONE',  ( -7.264118654998712010, 4.945491722146219793, -7.907633014911223945 ) ) ;
#5465 = DIRECTION ( 'NONE',  ( 0.000000000000000000, 0.000000000000000000, 1.000000000000000000 ) ) ;
#5466 = DIRECTION ( 'NONE',  ( 0.4999999999999976685, 0.8660254037844399289, 0.000000000000000000 ) ) ;
#5467 = ADVANCED_FACE ( 'NONE', ( #11034 ), #10800, .F. ) ;
#5468 = CARTESIAN_POINT ( 'NONE',  ( 0.000000000000000000, -20.00000000000000000, 0.000000000000000000 ) ) ;
#5469 = DIRECTION ( 'NONE',  ( -0.000000000000000000, -1.000000000000000000, -0.000000000000000000 ) ) ;
#5470 = CYLINDRICAL_SURFACE ( 'NONE', #6954, 5.000000000000000000 ) ;
#5471 = PRODUCT_DEFINITION_SHAPE ( 'NONE', 'NONE',  #15995 ) ;
#5472 = CARTESIAN_POINT ( 'NONE',  ( 5.200000000000002842, 0.000000000000000000, 0.000000000000000000 ) ) ;
#5473 = FACE_OUTER_BOUND ( 'NONE', #12436, .T. ) ;
#5474 = VECTOR ( 'NONE', #5985, 1000.000000000000000 ) ;
#5475 = DIRECTION ( 'NONE',  ( 0.000000000000000000, 0.000000000000000000, 1.000000000000000000 ) ) ;
#5476 = CARTESIAN_POINT ( 'NONE',  ( 4.458734124999999437, -22.50000000136559208, 1.846868145590737864 ) ) ;
#5477 = CARTESIAN_POINT ( 'NONE',  ( -3.033343224707664376, 3.753672977998667726, -7.249999998634409692 ) ) ;
#5478 = ORIENTED_EDGE ( 'NONE', *, *, #953, .T. ) ;
#5479 = CARTESIAN_POINT ( 'NONE',  ( 0.000000000000000000, -13.00000000000000178, -5.000000000000000000 ) ) ;
#5480 = ORIENTED_EDGE ( 'NONE', *, *, #9158, .F. ) ;
#5481 = ORIENTED_EDGE ( 'NONE', *, *, #9501, .T. ) ;
#5482 = VERTEX_POINT ( 'NONE', #7318 ) ;
#5483 = CARTESIAN_POINT ( 'NONE',  ( -4.458734125000000326, -30.25000000136559564, -1.846868145590735644 ) ) ;
#5484 = ADVANCED_FACE ( 'NONE', ( #5866 ), #15332, .F. ) ;
#5485 = CARTESIAN_POINT ( 'NONE',  ( 2.855764796983346177, -2.970025579236428737, -0.09382832055446485575 ) ) ;
#5486 = ORIENTED_EDGE ( 'NONE', *, *, #4747, .F. ) ;
#5487 = DIRECTION ( 'NONE',  ( 0.000000000000000000, 0.000000000000000000, -1.000000000000000000 ) ) ;
#5488 = CARTESIAN_POINT ( 'NONE',  ( 5.200000000000002842, 3.306546357697854719E-16, 2.700000000000001066 ) ) ;
#5489 = CARTESIAN_POINT ( 'NONE',  ( -4.276409079477644148, -1.261996585732578335, -4.812499998634405252 ) ) ;
#5490 = CARTESIAN_POINT ( 'NONE',  ( -4.391654775818395251, 2.390265326283148806, -5.499999997268814944 ) ) ;
#5491 = CARTESIAN_POINT ( 'NONE',  ( 2.071067811865475505, -26.81250000000000000, -5.000000000000000888 ) ) ;
#5492 = CARTESIAN_POINT ( 'NONE',  ( -2.131511515620587272, -3.916244202832140253, -6.687499998634407028 ) ) ;
#5493 = DIRECTION ( 'NONE',  ( -6.938893903907228378E-16, -1.000000000000000000, 0.000000000000000000 ) ) ;
#5494 = DIRECTION ( 'NONE',  ( -0.000000000000000000, -1.000000000000000000, -0.000000000000000000 ) ) ;
#5495 = CARTESIAN_POINT ( 'NONE',  ( -5.000000000000000000, -25.62500000273118417, -6.123233995736766282E-16 ) ) ;
#5496 = FACE_OUTER_BOUND ( 'NONE', #14570, .T. ) ;
#5497 = CARTESIAN_POINT ( 'NONE',  ( -4.458734125000000326, -26.87500000136559919, 1.846868145590734089 ) ) ;
#5498 = DIRECTION ( 'NONE',  ( 0.000000000000000000, 0.000000000000000000, 1.000000000000000000 ) ) ;
#5499 = ORIENTED_EDGE ( 'NONE', *, *, #3853, .F. ) ;
#5500 = ORIENTED_EDGE ( 'NONE', *, *, #15495, .T. ) ;
#5501 = CARTESIAN_POINT ( 'NONE',  ( 2.500000000000000000, 1.768423874527822681, -1.021000000000002794 ) ) ;
#5502 = CIRCLE ( 'NONE', #345, 2.649999999999985700 ) ;
#5504 = ORIENTED_EDGE ( 'NONE', *, *, #8743, .T. ) ;
#5503 = EDGE_CURVE ( 'NONE', #1672, #12917, #6663, .T. ) ;
#5505 = AXIS2_PLACEMENT_3D ( 'NONE', #2063, #8228, #13126 ) ;
#5506 = DIRECTION ( 'NONE',  ( 0.000000000000000000, 0.000000000000000000, 1.000000000000000000 ) ) ;
#5507 = EDGE_CURVE ( 'NONE', #9005, #11530, #1743, .T. ) ;
#5508 = ORIENTED_EDGE ( 'NONE', *, *, #7307, .F. ) ;
#5509 = CARTESIAN_POINT ( 'NONE',  ( 7.908030677224555660, -3.059924800338350792, -7.792662696733365202 ) ) ;
#5510 = CARTESIAN_POINT ( 'NONE',  ( -21.01110699893060030, -1.230770033143087371E-15, 33.74230484541325126 ) ) ;
#5511 = CARTESIAN_POINT ( 'NONE',  ( -1.846868145590737420, -26.00000000136559564, 4.458734124999999437 ) ) ;
#5512 = CARTESIAN_POINT ( 'NONE',  ( -5.000000000000002665, 1.292545281756915047E-15, -0.4202630448617610814 ) ) ;
#5513 = CARTESIAN_POINT ( 'NONE',  ( -90.00000000000000000, -35.00000000000000711, -7.500000000000000000 ) ) ;
#5514 = CONTEXT_DEPENDENT_SHAPE_REPRESENTATION ( #2163, #12203 ) ;
#5515 = CARTESIAN_POINT ( 'NONE',  ( 5.000000000000000888, -31.93750000000000000, -2.071067811865475505 ) ) ;
#5516 = CARTESIAN_POINT ( 'NONE',  ( -41.99999999999978684, -9.000000000000001776, -1.500000000000000888 ) ) ;
#5517 = EDGE_LOOP ( 'NONE', ( #4779, #7091, #3818, #9863 ) ) ;
#5518 = AXIS2_PLACEMENT_3D ( 'NONE', #6770, #15339, #15421 ) ;
#5519 = SURFACE_STYLE_FILL_AREA ( #3402 ) ;
#5520 = ORIENTED_EDGE ( 'NONE', *, *, #3334, .T. ) ;
#5521 = CARTESIAN_POINT ( 'NONE',  ( -7.169303301815265428, 4.521054846639298574, -7.349897473155284189 ) ) ;
#5522 = EDGE_CURVE ( 'NONE', #10564, #8217, #974, .T. ) ;
#5523 = ORIENTED_EDGE ( 'NONE', *, *, #15764, .F. ) ;
#5524 = VECTOR ( 'NONE', #15556, 1000.000000000000000 ) ;
#5525 = CARTESIAN_POINT ( 'NONE',  ( 0.000000000000000000, 40.00000000000000000, 0.000000000000000000 ) ) ;
#5526 = CARTESIAN_POINT ( 'NONE',  ( 0.000000000000000000, 0.000000000000000000, -4.974599999999998801 ) ) ;
#5527 = CARTESIAN_POINT ( 'NONE',  ( -4.276409079477644148, -1.261996585732578335, 0.9375000013655925279 ) ) ;
#5528 = CYLINDRICAL_SURFACE ( 'NONE', #2849, 2.649999999999992806 ) ;
#5529 = CARTESIAN_POINT ( 'NONE',  ( -4.999999999999849898, 1.272547481429008309, -1.586597482644648505 ) ) ;
#5530 = CARTESIAN_POINT ( 'NONE',  ( -60.00000000000000000, 0.000000000000000000, -18.00000000000001066 ) ) ;
#5531 = ORIENTED_EDGE ( 'NONE', *, *, #2172, .T. ) ;
#5532 = CARTESIAN_POINT ( 'NONE',  ( 7.500000000000000000, 2.932633423934446260, -0.4709827563909316783 ) ) ;
#5533 = DIRECTION ( 'NONE',  ( -1.000000000000000000, -0.000000000000000000, -0.000000000000000000 ) ) ;
#5534 =( GEOMETRIC_REPRESENTATION_CONTEXT ( 3 ) GLOBAL_UNCERTAINTY_ASSIGNED_CONTEXT ( ( #13845 ) ) GLOBAL_UNIT_ASSIGNED_CONTEXT ( ( #10499, #4428, #5644 ) ) REPRESENTATION_CONTEXT ( 'NONE', 'WORKASPACE' ) );
#5535 = CARTESIAN_POINT ( 'NONE',  ( -5.000000000000000888, -26.68750000273119127, -2.071067811865475949 ) ) ;
#5536 = ADVANCED_FACE ( 'NONE', ( #14318 ), #9160, .T. ) ;
#5537 = EDGE_LOOP ( 'NONE', ( #15900, #14927, #5486, #2397, #5788 ) ) ;
#5538 = CARTESIAN_POINT ( 'NONE',  ( -39.99999999999999289, -13.00000000000000178, 8.300651832549021947E-13 ) ) ;
#5539 = ORIENTED_EDGE ( 'NONE', *, *, #600, .T. ) ;
#5540 = EDGE_CURVE ( 'NONE', #14394, #637, #10587, .T. ) ;
#5541 = CIRCLE ( 'NONE', #7615, 2.649999999999992806 ) ;
#5542 = ORIENTED_EDGE ( 'NONE', *, *, #13940, .T. ) ;
#5543 = CARTESIAN_POINT ( 'NONE',  ( -5.000000000000000000, -30.50000000000000000, -6.123233995736766282E-16 ) ) ;
#5544 = DIRECTION ( 'NONE',  ( 0.000000000000000000, 0.000000000000000000, -1.000000000000000000 ) ) ;
#5545 = CARTESIAN_POINT ( 'NONE',  ( -7.500000000000006217, 0.7513028741560140444, -0.02472015219303315067 ) ) ;
#5546 =( GEOMETRIC_REPRESENTATION_CONTEXT ( 3 ) GLOBAL_UNCERTAINTY_ASSIGNED_CONTEXT ( ( #2852 ) ) GLOBAL_UNIT_ASSIGNED_CONTEXT ( ( #5957, #14593, #7256 ) ) REPRESENTATION_CONTEXT ( 'NONE', 'WORKASPACE' ) );
#5547 = DIRECTION ( 'NONE',  ( 0.4999999999999997224, 0.000000000000000000, 0.8660254037844388186 ) ) ;
#5548 = DIRECTION ( 'NONE',  ( 0.5000000000000022204, 0.8660254037844374864, -0.000000000000000000 ) ) ;
#5549 = VECTOR ( 'NONE', #11436, 999.9999999999998863 ) ;
#5550 = DIRECTION ( 'NONE',  ( -1.000000000000000000, -0.000000000000000000, -0.000000000000000000 ) ) ;
#5551 = LINE ( 'NONE', #4342, #6910 ) ;
#5552 = CARTESIAN_POINT ( 'NONE',  ( -28.86751345948129455, -3.000000000000000000, 49.99999999999999289 ) ) ;
#5553 = CARTESIAN_POINT ( 'NONE',  ( 25.00000000000000000, 0.000000000000000000, 0.000000000000000000 ) ) ;
#5554 = CARTESIAN_POINT ( 'NONE',  ( -1.846868145590737420, -21.75000000136559564, 4.458734124999999437 ) ) ;
#5555 = CARTESIAN_POINT ( 'NONE',  ( 4.799145180956616130, -0.5093500532425063732, -0.3749999986344090264 ) ) ;
#5556 = ORIENTED_EDGE ( 'NONE', *, *, #8574, .T. ) ;
#5557 = CARTESIAN_POINT ( 'NONE',  ( 35.00000000000000000, 37.00000000000000000, 5.999999999999991118 ) ) ;
#5558 = ORIENTED_EDGE ( 'NONE', *, *, #15347, .F. ) ;
#5559 = ORIENTED_EDGE ( 'NONE', *, *, #7377, .F. ) ;
#5560 = COLOUR_RGB ( '', 0.09019608, 0.27058824, 0.51372549) ;
#5561 = ADVANCED_FACE ( 'NONE', ( #15542 ), #8036, .F. ) ;
#5563 = PRESENTATION_LAYER_ASSIGNMENT (  '', '', ( #9173 ) ) ;
#5562 =( NAMED_UNIT ( * ) SI_UNIT ( $, .STERADIAN. ) SOLID_ANGLE_UNIT ( ) );
#5564 = CARTESIAN_POINT ( 'NONE',  ( 4.458734125000000326, -25.62500000136559564, -1.846868145590734978 ) ) ;
#5565 = CARTESIAN_POINT ( 'NONE',  ( -1.391697335622809950, -4.043246145443391448, -3.503898532754372575 ) ) ;
#5566 = CIRCLE ( 'NONE', #14582, 4.000000000000000000 ) ;
#5567 = ORIENTED_EDGE ( 'NONE', *, *, #1571, .F. ) ;
#5568 = CARTESIAN_POINT ( 'NONE',  ( 1.415196051561583790, -4.795541693661363958, -6.250000000000001776 ) ) ;
#5569 = CARTESIAN_POINT ( 'NONE',  ( 45.58845726811988897, 88.59290746114278647, 42.96152422706634155 ) ) ;
#5570 = CARTESIAN_POINT ( 'NONE',  ( -1.261996585732579224, 4.276409079477648589, -6.062499998634407028 ) ) ;
#5571 = CARTESIAN_POINT ( 'NONE',  ( 2.602085213965210642E-15, 8.660254037844392627, -1.000000000000000888 ) ) ;
#5572 = CARTESIAN_POINT ( 'NONE',  ( 3.535533905932736864, -25.12500000000000000, 3.535533905932738641 ) ) ;
#5573 = CIRCLE ( 'NONE', #918, 2.499999999999998668 ) ;
#5574 = CARTESIAN_POINT ( 'NONE',  ( -3.753672977998669946, -3.033343224707661712, -6.749999998634408804 ) ) ;
#5575 = FACE_OUTER_BOUND ( 'NONE', #11433, .T. ) ;
#5576 = DIRECTION ( 'NONE',  ( -1.000000000000000000, 0.000000000000000000, 0.000000000000000000 ) ) ;
#5577 = CARTESIAN_POINT ( 'NONE',  ( 2.071067811865475505, -25.93750000273118772, -5.000000000000000888 ) ) ;
#5578 = AXIS2_PLACEMENT_3D ( 'NONE', #2748, #14064, #9150 ) ;
#5579 = ORIENTED_EDGE ( 'NONE', *, *, #13823, .T. ) ;
#5580 = CIRCLE ( 'NONE', #9652, 4.000000000000000000 ) ;
#5581 = CARTESIAN_POINT ( 'NONE',  ( 1.846868145590736310, -24.62500000136559564, 4.458734124999997661 ) ) ;
#5582 = CARTESIAN_POINT ( 'NONE',  ( 5.000000000000004441, -2.247904837838113790E-16, -7.045263047592947636 ) ) ;
#5583 = ORIENTED_EDGE ( 'NONE', *, *, #5117, .T. ) ;
#5584 = EDGE_LOOP ( 'NONE', ( #7819, #735, #15524, #7576 ) ) ;
#5585 = DIRECTION ( 'NONE',  ( 0.000000000000000000, 0.000000000000000000, 1.000000000000000000 ) ) ;
#5586 = AXIS2_PLACEMENT_3D ( 'NONE', #11296, #247, #8880 ) ;
#5587 = ORIENTED_EDGE ( 'NONE', *, *, #3647, .T. ) ;
#5588 = CYLINDRICAL_SURFACE ( 'NONE', #1916, 39.99999999999999289 ) ;
#5589 = AXIS2_PLACEMENT_3D ( 'NONE', #4353, #8248, #9291 ) ;
#5590 = CARTESIAN_POINT ( 'NONE',  ( 40.89003422689814471, -3.000000000000000000, -27.08062585941929967 ) ) ;
#5591 = CARTESIAN_POINT ( 'NONE',  ( 2.730187237215162345E-16, -29.43750000136559208, -4.458734124999999437 ) ) ;
#5592 = LINE ( 'NONE', #4212, #15805 ) ;
#5593 = EDGE_CURVE ( 'NONE', #3963, #1816, #14286, .T. ) ;
#5594 = VECTOR ( 'NONE', #8053, 1000.000000000000000 ) ;
#5595 = DIRECTION ( 'NONE',  ( 0.8660254037844410391, -0.4999999999999958367, 0.000000000000000000 ) ) ;
#5596 = CARTESIAN_POINT ( 'NONE',  ( 5.000000000000000000, -32.00000000000000000, 0.000000000000000000 ) ) ;
#5597 = LINE ( 'NONE', #1711, #10011 ) ;
#5598 = VERTEX_POINT ( 'NONE', #4134 ) ;
#5599 = CIRCLE ( 'NONE', #13841, 2.499999999999998668 ) ;
#5600 = VERTEX_POINT ( 'NONE', #13986 ) ;
#5601 = CARTESIAN_POINT ( 'NONE',  ( 0.2779000157839381924, 8.820699686765076208, -7.928862157988310955 ) ) ;
#5602 = ORIENTED_EDGE ( 'NONE', *, *, #5827, .T. ) ;
#5603 = ADVANCED_FACE ( 'NONE', ( #5439 ), #3002, .T. ) ;
#5604 = AXIS2_PLACEMENT_3D ( 'NONE', #8459, #8539, #10943 ) ;
#5605 = SURFACE_STYLE_FILL_AREA ( #10381 ) ;
#5606 = CARTESIAN_POINT ( 'NONE',  ( -5.000000000000000888, -27.68750000273119127, -2.071067811865475949 ) ) ;
#5607 = CARTESIAN_POINT ( 'NONE',  ( 39.54732521363962405, -4.732646668676187218, 28.47097061891900438 ) ) ;
#5608 = ADVANCED_FACE ( 'NONE', ( #3399, #7217 ), #9698, .F. ) ;
#5609 = DIRECTION ( 'NONE',  ( 1.000000000000000000, 0.000000000000000000, 0.000000000000000000 ) ) ;
#5610 = EDGE_CURVE ( 'NONE', #12513, #3779, #8281, .T. ) ;
#5611 = CARTESIAN_POINT ( 'NONE',  ( 3.401574460001763001, -4.209348295687703967, -7.062499997268814944 ) ) ;
#5612 = DIRECTION ( 'NONE',  ( -0.8660254037844385966, 0.000000000000000000, -0.5000000000000000000 ) ) ;
#5613 = VECTOR ( 'NONE', #6021, 1000.000000000000114 ) ;
#5614 = CARTESIAN_POINT ( 'NONE',  ( 4.795541693661363958, 1.415196051561583790, -2.000000000000001776 ) ) ;
#5615 = DIRECTION ( 'NONE',  ( -0.000000000000000000, -0.000000000000000000, 1.000000000000000000 ) ) ;
#5616 = VERTEX_POINT ( 'NONE', #3331 ) ;
#5617 = CARTESIAN_POINT ( 'NONE',  ( -39.99999999999999289, -9.000000000000001776, -2.500000000000079492 ) ) ;
#5618 = CARTESIAN_POINT ( 'NONE',  ( -5.000000000000004441, -7.530481206757679743E-15, -2.420263044861759472 ) ) ;
#5619 = ORIENTED_EDGE ( 'NONE', *, *, #12684, .F. ) ;
#5620 = DIRECTION ( 'NONE',  ( 0.000000000000000000, 0.5000000000000012212, 0.8660254037844380415 ) ) ;
#5621 = ORIENTED_EDGE ( 'NONE', *, *, #8865, .F. ) ;
#5622 = VERTEX_POINT ( 'NONE', #8349 ) ;
#5623 = DIRECTION ( 'NONE',  ( 0.000000000000000000, 1.000000000000000000, -1.287488025362403787E-15 ) ) ;
#5624 = DIRECTION ( 'NONE',  ( 1.000000000000000000, 0.000000000000000000, -0.000000000000000000 ) ) ;
#5625 = CARTESIAN_POINT ( 'NONE',  ( -7.500000000000005329, 4.330127018922194537, -0.9999999999999974465 ) ) ;
#5626 = AXIS2_PLACEMENT_3D ( 'NONE', #1846, #10424, #2010 ) ;
#5627 = EDGE_CURVE ( 'NONE', #2457, #8017, #8514, .T. ) ;
#5628 = CARTESIAN_POINT ( 'NONE',  ( -9.184850993605147944E-16, -31.25000000000000000, 5.000000000000000000 ) ) ;
#5629 = CARTESIAN_POINT ( 'NONE',  ( -5.000000000000000888, -25.43750000000000355, 2.071067811865474617 ) ) ;
#5630 = ADVANCED_FACE ( 'NONE', ( #15937 ), #13244, .T. ) ;
#5631 = DIRECTION ( 'NONE',  ( 0.000000000000000000, 0.000000000000000000, 1.000000000000000000 ) ) ;
#5632 = VECTOR ( 'NONE', #9, 1000.000000000000000 ) ;
#5633 = CARTESIAN_POINT ( 'NONE',  ( -10.39117206796836079, 1.272551561242683567E-15, -8.499999999999996447 ) ) ;
#5634 = CARTESIAN_POINT ( 'NONE',  ( 23.49999999999956657, -8.782289339527253835E-13, 1.500000000000000000 ) ) ;
#5635 = LINE ( 'NONE', #10578, #15704 ) ;
#5636 = CARTESIAN_POINT ( 'NONE',  ( 2.730187237215162345E-16, -30.43750000136559564, -4.458734124999999437 ) ) ;
#5637 = CARTESIAN_POINT ( 'NONE',  ( -1.261996585732579224, 4.276409079477648589, -1.062499998634405696 ) ) ;
#5638 = ORIENTED_EDGE ( 'NONE', *, *, #15597, .T. ) ;
#5639 = UNCERTAINTY_MEASURE_WITH_UNIT (LENGTH_MEASURE( 1.000000000000000082E-05 ), #2925, 'distance_accuracy_value', 'NONE');
#5640 = LINE ( 'NONE', #4657, #11760 ) ;
#5641 = ORIENTED_EDGE ( 'NONE', *, *, #8244, .T. ) ;
#5642 = VERTEX_POINT ( 'NONE', #4775 ) ;
#5643 = VECTOR ( 'NONE', #5195, 1000.000000000000000 ) ;
#5644 =( NAMED_UNIT ( * ) SI_UNIT ( $, .STERADIAN. ) SOLID_ANGLE_UNIT ( ) );
#5645 = CARTESIAN_POINT ( 'NONE',  ( -3.152801135295367985, -28.06250000136559564, 3.152801135295367096 ) ) ;
#5646 = LINE ( 'NONE', #15513, #5061 ) ;
#5647 = CIRCLE ( 'NONE', #9522, 2.041999999999999815 ) ;
#5648 = CARTESIAN_POINT ( 'NONE',  ( 25.00000000000000000, 0.000000000000000000, 0.000000000000000000 ) ) ;
#5649 = CARTESIAN_POINT ( 'NONE',  ( 0.000000000000000000, 2.357898499370433054, -1.951563910473907981E-15 ) ) ;
#5650 = CARTESIAN_POINT ( 'NONE',  ( 4.799145180956616130, -0.5093500532425063732, -4.374999998634405252 ) ) ;
#5651 = CARTESIAN_POINT ( 'NONE',  ( 3.007492831193109062, -2.999999999999999556, 48.95212133182432268 ) ) ;
#5652 = AXIS2_PLACEMENT_3D ( 'NONE', #4850, #11949, #12262 ) ;
#5653 = ADVANCED_FACE ( 'NONE', ( #15619 ), #14637, .F. ) ;
#5654 = CARTESIAN_POINT ( 'NONE',  ( -9.184850993605147944E-16, -26.25000000000000355, 5.000000000000000000 ) ) ;
#5655 = CARTESIAN_POINT ( 'NONE',  ( 4.276409079477644148, 1.261996585732577891, -6.312499998634407028 ) ) ;
#5656 = CYLINDRICAL_SURFACE ( 'NONE', #12482, 5.000000000000000000 ) ;
#5657 = DIRECTION ( 'NONE',  ( 0.000000000000000000, 0.000000000000000000, 1.000000000000000000 ) ) ;
#5658 = CARTESIAN_POINT ( 'NONE',  ( -4.458734124999999437, -30.93750000136559564, -5.460374474430324690E-16 ) ) ;
#5659 = EDGE_LOOP ( 'NONE', ( #10325, #12552, #13769, #13014 ) ) ;
#5660 = AXIS2_PLACEMENT_3D ( 'NONE', #5966, #9668, #5307 ) ;
#5661 = CARTESIAN_POINT ( 'NONE',  ( -1.846868145590737420, -27.75000000136559564, 4.458734124999997661 ) ) ;
#5662 = CARTESIAN_POINT ( 'NONE',  ( 6.486836893983276120, -4.915077010913956101, -7.231838333420564702 ) ) ;
#5663 = ORIENTED_EDGE ( 'NONE', *, *, #3647, .F. ) ;
#5664 = VERTEX_POINT ( 'NONE', #2183 ) ;
#5665 = CARTESIAN_POINT ( 'NONE',  ( 2.805705207896068476, -3.226868319750173075, -3.503898532754370354 ) ) ;
#5666 = DIRECTION ( 'NONE',  ( -0.5000000000000005551, 0.000000000000000000, 0.8660254037844383745 ) ) ;
#5667 = VERTEX_POINT ( 'NONE', #11955 ) ;
#5669 = CIRCLE ( 'NONE', #9792, 5.560781378645573980 ) ;
#5668 = CARTESIAN_POINT ( 'NONE',  ( -60.00000000000000000, -5.000000000000004441, 17.99999999999999289 ) ) ;
#5670 = CARTESIAN_POINT ( 'NONE',  ( -4.000000000000000888, -2.309401076758512694, -3.504269196027526512 ) ) ;
#5671 = EDGE_CURVE ( 'NONE', #11827, #6744, #9496, .T. ) ;
#5672 = CARTESIAN_POINT ( 'NONE',  ( -4.458734125000001214, -29.12500000136559919, 1.846868145590734089 ) ) ;
#5673 = CARTESIAN_POINT ( 'NONE',  ( 1.287237434362044075, 3.875615274277557809, -3.430618716626812059 ) ) ;
#5674 =( REPRESENTATION_RELATIONSHIP ('NONE','NONE', #4176, #14733 ) REPRESENTATION_RELATIONSHIP_WITH_TRANSFORMATION ( #11565 )SHAPE_REPRESENTATION_RELATIONSHIP( ) );
#5675 = CARTESIAN_POINT ( 'NONE',  ( -5.000000000000004441, -1.011557177027151181E-15, -4.545263047592944083 ) ) ;
#5676 = PRODUCT_CONTEXT ( 'NONE', #7320, 'mechanical' ) ;
#5677 = CARTESIAN_POINT ( 'NONE',  ( 6.874999999999997335, -4.690970937165719334, -7.298562697733109061 ) ) ;
#5678 = CYLINDRICAL_SURFACE ( 'NONE', #14145, 2.000000000000000888 ) ;
#5679 = ORIENTED_EDGE ( 'NONE', *, *, #14762, .T. ) ;
#5680 = EDGE_LOOP ( 'NONE', ( #10520, #6094, #2965, #7613 ) ) ;
#5681 = DIRECTION ( 'NONE',  ( -1.000000000000000000, 0.000000000000000000, -3.343241100358131282E-16 ) ) ;
#5682 = EDGE_LOOP ( 'NONE', ( #5856, #8565, #5697, #359 ) ) ;
#5683 = EDGE_CURVE ( 'NONE', #6058, #8136, #7287, .T. ) ;
#5684 = CARTESIAN_POINT ( 'NONE',  ( -4.999999999999844569, 1.272547481429019856, -4.586597482644648949 ) ) ;
#5685 = CARTESIAN_POINT ( 'NONE',  ( -5.000000000000004441, -7.530481206757679743E-15, -3.420263044861759916 ) ) ;
#5686 = LINE ( 'NONE', #606, #10526 ) ;
#5687 = CARTESIAN_POINT ( 'NONE',  ( 3.753672977998667726, 3.033343224707664376, 0.5000000013655936382 ) ) ;
#5688 = DIRECTION ( 'NONE',  ( -0.000000000000000000, -0.000000000000000000, -1.000000000000000000 ) ) ;
#5689 = LINE ( 'NONE', #4151, #1238 ) ;
#5690 = CARTESIAN_POINT ( 'NONE',  ( -35.00000000000000000, 40.00000000000000000, 2.649999999999992806 ) ) ;
#5691 = ORIENTED_EDGE ( 'NONE', *, *, #15137, .T. ) ;
#5692 = CARTESIAN_POINT ( 'NONE',  ( 7.500000000000000000, 0.7513028741560167090, -0.02472015219302843916 ) ) ;
#5693 = DIRECTION ( 'NONE',  ( 1.000000000000000000, 1.734723475976808080E-15, 0.000000000000000000 ) ) ;
#5694 = DIRECTION ( 'NONE',  ( 0.000000000000000000, 0.000000000000000000, -1.000000000000000000 ) ) ;
#5695 = EDGE_LOOP ( 'NONE', ( #11492, #9511 ) ) ;
#5696 = CARTESIAN_POINT ( 'NONE',  ( 5.000000000000000888, -26.93750000000000355, -2.071067811865475505 ) ) ;
#5697 = ORIENTED_EDGE ( 'NONE', *, *, #8121, .F. ) ;
#5698 = ORIENTED_EDGE ( 'NONE', *, *, #9017, .F. ) ;
#5699 = CARTESIAN_POINT ( 'NONE',  ( 5.000000000000000888, -23.06250000273119127, -2.071067811865475505 ) ) ;
#5700 = ADVANCED_FACE ( 'NONE', ( #1055 ), #9550, .F. ) ;
#5701 = CARTESIAN_POINT ( 'NONE',  ( -1.243802165048909503, 3.900692638707381921, -3.223146290109805800 ) ) ;
#5702 = EDGE_CURVE ( 'NONE', #12489, #8029, #5963, .T. ) ;
#5703 = CARTESIAN_POINT ( 'NONE',  ( 4.000000000000000000, 2.309401076758497151, -3.433295621305379353 ) ) ;
#5704 = DIRECTION ( 'NONE',  ( -0.000000000000000000, 1.000000000000000000, -0.000000000000000000 ) ) ;
#5705 = LINE ( 'NONE', #857, #14270 ) ;
#5706 = CARTESIAN_POINT ( 'NONE',  ( 3.535533905932736864, -23.12500000000000000, 3.535533905932738641 ) ) ;
#5707 = CARTESIAN_POINT ( 'NONE',  ( -36.99999999999999289, -13.00000000000000178, 2.000000000000830891 ) ) ;
#5708 = CARTESIAN_POINT ( 'NONE',  ( -35.00000000000000000, 40.00000000000000000, -2.649999999999992806 ) ) ;
#5709 = FACE_OUTER_BOUND ( 'NONE', #7700, .T. ) ;
#5710 = CARTESIAN_POINT ( 'NONE',  ( 2.730187237215162345E-16, -31.43750000136559564, -4.458734124999999437 ) ) ;
#5711 = CARTESIAN_POINT ( 'NONE',  ( -4.799145180956616130, 0.5093500532425063732, -1.874999998634406584 ) ) ;
#5712 = ORIENTED_EDGE ( 'NONE', *, *, #312, .F. ) ;
#5713 = FACE_OUTER_BOUND ( 'NONE', #3265, .T. ) ;
#5714 = ORIENTED_EDGE ( 'NONE', *, *, #7348, .T. ) ;
#5715 = ORIENTED_EDGE ( 'NONE', *, *, #9553, .T. ) ;
#5716 = CARTESIAN_POINT ( 'NONE',  ( -3.152801135295367096, -26.31250000136559564, -3.152801135295367541 ) ) ;
#5717 = CARTESIAN_POINT ( 'NONE',  ( 5.000000000000000000, -31.56250000136559564, 0.000000000000000000 ) ) ;
#5718 = EDGE_CURVE ( 'NONE', #7037, #7701, #7960, .T. ) ;
#5719 = DIRECTION ( 'NONE',  ( 0.000000000000000000, -1.000000000000000000, 0.000000000000000000 ) ) ;
#5720 = CARTESIAN_POINT ( 'NONE',  ( 2.500000000000000000, -1.178949249685213863, 2.042000000000002924 ) ) ;
#5721 = CARTESIAN_POINT ( 'NONE',  ( 4.799145180956616130, -0.5093500532425063732, -5.374999998634405252 ) ) ;
#5722 = FACE_OUTER_BOUND ( 'NONE', #15453, .T. ) ;
#5723 = AXIS2_PLACEMENT_3D ( 'NONE', #13317, #4384, #4688 ) ;
#5724 = CARTESIAN_POINT ( 'NONE',  ( 3.535533905932738197, -24.87500000000000000, -3.535533905932738197 ) ) ;
#5725 = CARTESIAN_POINT ( 'NONE',  ( -0.5093500532425060401, -4.799145180956616130, -7.624999998634408804 ) ) ;
#5726 = CARTESIAN_POINT ( 'NONE',  ( -5.000000000000004441, -1.011557177027151181E-15, -3.545263047592942307 ) ) ;
#5727 = CARTESIAN_POINT ( 'NONE',  ( -124.9999999999999716, -115.2072594216370049, 7.500000000000001776 ) ) ;
#5728 = CARTESIAN_POINT ( 'NONE',  ( 1.846868145590735200, -29.25000000136559564, -4.458734125000000326 ) ) ;
#5729 = ORIENTED_EDGE ( 'NONE', *, *, #15736, .F. ) ;
#5730 = CARTESIAN_POINT ( 'NONE',  ( 2.730187237215162345E-16, -24.18750000136559564, -4.458734124999999437 ) ) ;
#5731 = FACE_OUTER_BOUND ( 'NONE', #4498, .T. ) ;
#5732 = ORIENTED_EDGE ( 'NONE', *, *, #9551, .F. ) ;
#5733 = EDGE_LOOP ( 'NONE', ( #13560, #5558, #9741, #13054 ) ) ;
#5734 = CARTESIAN_POINT ( 'NONE',  ( -7.500000000000005329, 4.330127018922194537, -9.999999999999998224 ) ) ;
#5735 = CARTESIAN_POINT ( 'NONE',  ( 3.152801135295366208, -28.56250000136559564, 3.152801135295367985 ) ) ;
#5736 = EDGE_CURVE ( 'NONE', #5642, #14864, #6143, .T. ) ;
#5737 = DIRECTION ( 'NONE',  ( -1.000000000000000000, -1.239088197126290324E-16, 0.000000000000000000 ) ) ;
#5738 = EDGE_CURVE ( 'NONE', #8282, #7835, #3043, .T. ) ;
#5739 = EDGE_CURVE ( 'NONE', #12769, #6058, #4692, .T. ) ;
#5740 =( BOUNDED_CURVE ( )  B_SPLINE_CURVE ( 2, ( #14419, #14654, #4711, #3345, #13183, #15870, #15722, #2118, #2285 ),
 .UNSPECIFIED., .F., .F. ) 
 B_SPLINE_CURVE_WITH_KNOTS ( ( 3, 2, 2, 2, 3 ),
 ( 0.8750000000000000000, 0.8874999999999999556, 0.8999999999999999112, 0.9124999999999998668, 0.9249999999999998224 ),
 .UNSPECIFIED. ) 
 CURVE ( )  GEOMETRIC_REPRESENTATION_ITEM ( )  RATIONAL_B_SPLINE_CURVE ( ( 1.000000000000000000, 0.9238795325112867385, 1.000000000000000000, 0.9238795325112867385, 1.000000000000000000, 0.9238795325112867385, 1.000000000000000000, 0.9238795325112880708, 0.9999999999999986677 ) ) 
 REPRESENTATION_ITEM ( '' )  );
#5741 = ORIENTED_EDGE ( 'NONE', *, *, #15328, .T. ) ;
#5742 = DIRECTION ( 'NONE',  ( 1.239088197126290324E-16, -1.000000000000000000, 0.000000000000000000 ) ) ;
#5743 = CARTESIAN_POINT ( 'NONE',  ( 40.27815445939820904, -3.253774389711718396, -27.73097106845637683 ) ) ;
#5744 = CARTESIAN_POINT ( 'NONE',  ( -3.152801135295367096, -29.31250000136559564, -3.152801135295367541 ) ) ;
#5745 = CARTESIAN_POINT ( 'NONE',  ( 1.390230914382191596, 4.043987460488659202, -3.502507215260488582 ) ) ;
#5746 = LINE ( 'NONE', #8111, #9281 ) ;
#5747 = AXIS2_PLACEMENT_3D ( 'NONE', #1624, #427, #15219 ) ;
#5748 = DIRECTION ( 'NONE',  ( -0.7071067811865306973, 8.659560562355138702E-17, -0.7071067811865643371 ) ) ;
#5749 = CIRCLE ( 'NONE', #14782, 60.00000000000000000 ) ;
#5750 = VERTEX_POINT ( 'NONE', #2266 ) ;
#5751 = EDGE_LOOP ( 'NONE', ( #2603, #11786, #8242, #11610, #4123 ) ) ;
#5752 = CARTESIAN_POINT ( 'NONE',  ( -5.276498195232070643, 6.073236878018064111, -7.633618187056732118 ) ) ;
#5753 = EDGE_CURVE ( 'NONE', #13811, #15784, #15854, .T. ) ;
#5754 = ORIENTED_EDGE ( 'NONE', *, *, #7419, .F. ) ;
#5755 = AXIS2_PLACEMENT_3D ( 'NONE', #7364, #10030, #9697 ) ;
#5756 = DIRECTION ( 'NONE',  ( -0.000000000000000000, -1.000000000000000000, -0.000000000000000000 ) ) ;
#5757 = FACE_OUTER_BOUND ( 'NONE', #558, .T. ) ;
#5758 = CARTESIAN_POINT ( 'NONE',  ( 3.916244202832140253, -2.131511515620588160, 1.562500001365592972 ) ) ;
#5759 = DIRECTION ( 'NONE',  ( 0.000000000000000000, -1.000000000000000000, 0.000000000000000000 ) ) ;
#5760 = CARTESIAN_POINT ( 'NONE',  ( -4.799145180956616130, 0.5093500532425063732, -0.1249999986344088321 ) ) ;
#5761 = CARTESIAN_POINT ( 'NONE',  ( -5.725490332117410652, -3.000000000000000000, 49.91684015347181003 ) ) ;
#5762 = CARTESIAN_POINT ( 'NONE',  ( 5.000000000000092371, 0.7223674278660651149, -2.021799365517154889 ) ) ;
#5763 = CARTESIAN_POINT ( 'NONE',  ( 2.071067811865462183, -25.18750000000000355, 5.000000000000013323 ) ) ;
#5764 = VERTEX_POINT ( 'NONE', #10998 ) ;
#5765 = CYLINDRICAL_SURFACE ( 'NONE', #990, 5.999999999999991118 ) ;
#5766 = CARTESIAN_POINT ( 'NONE',  ( -6.765421556309547668E-13, 50.00000000000000000, 67.49999999999930367 ) ) ;
#5767 = CYLINDRICAL_SURFACE ( 'NONE', #15624, 2.500000000000000444 ) ;
#5768 = ORIENTED_EDGE ( 'NONE', *, *, #14393, .F. ) ;
#5769 = CARTESIAN_POINT ( 'NONE',  ( 19.99999999999956657, -8.786575603324269439E-13, -6.000000000000000000 ) ) ;
#5770 = ORIENTED_EDGE ( 'NONE', *, *, #4129, .F. ) ;
#5771 = EDGE_LOOP ( 'NONE', ( #5852, #1815, #10324 ) ) ;
#5772 = CARTESIAN_POINT ( 'NONE',  ( 3.061616997868383141E-16, -22.87500000273118772, -5.000000000000000000 ) ) ;
#5773 = LINE ( 'NONE', #13659, #14626 ) ;
#5774 = CARTESIAN_POINT ( 'NONE',  ( 3.999999999999999112, -1.539600717839012978, -3.300726591567080703 ) ) ;
#5775 =( REPRESENTATION_RELATIONSHIP ('NONE','NONE', #4176, #1906 ) REPRESENTATION_RELATIONSHIP_WITH_TRANSFORMATION ( #12952 )SHAPE_REPRESENTATION_RELATIONSHIP( ) );
#5776 = CARTESIAN_POINT ( 'NONE',  ( 2.500000000000000000, -1.178949249685213863, 2.042000000000002924 ) ) ;
#5777 = PLANE ( 'NONE',  #1618 ) ;
#5778 = CARTESIAN_POINT ( 'NONE',  ( 0.000000000000000000, -11.00000000000000178, -6.000000000000000888 ) ) ;
#5779 = CARTESIAN_POINT ( 'NONE',  ( -4.209348295687703967, -3.401574460001763001, -7.437500000000004441 ) ) ;
#5780 = DIRECTION ( 'NONE',  ( 0.4999999999999961697, 0.000000000000000000, -0.8660254037844409281 ) ) ;
#5781 = ADVANCED_FACE ( 'NONE', ( #7365 ), #92, .T. ) ;
#5782 = CARTESIAN_POINT ( 'NONE',  ( 3.061616997868383141E-16, -22.87500000273118772, -5.000000000000000000 ) ) ;
#5783 = CARTESIAN_POINT ( 'NONE',  ( 3.152801135295366208, -27.81250000136559564, 3.152801135295367985 ) ) ;
#5784 = VECTOR ( 'NONE', #1845, 1000.000000000000000 ) ;
#5785 = CARTESIAN_POINT ( 'NONE',  ( -2.131511515620587272, -3.916244202832140253, -1.687499998634406362 ) ) ;
#5786 = ORIENTED_EDGE ( 'NONE', *, *, #8574, .F. ) ;
#5787 = CARTESIAN_POINT ( 'NONE',  ( 3.080866544135724361, 6.881514909250313394, -7.026396753507434312 ) ) ;
#5788 = ORIENTED_EDGE ( 'NONE', *, *, #4164, .T. ) ;
#5789 = ORIENTED_EDGE ( 'NONE', *, *, #15734, .F. ) ;
#5790 = PRESENTATION_STYLE_ASSIGNMENT (( #871 ) ) ;
#5791 = ORIENTED_EDGE ( 'NONE', *, *, #312, .T. ) ;
#5792 = CARTESIAN_POINT ( 'NONE',  ( -4.458734125000000326, -26.25000000136559208, -1.846868145590735644 ) ) ;
#5793 = CARTESIAN_POINT ( 'NONE',  ( 3.061616997868383043E-15, 40.00000000000000000, -25.00000000000000000 ) ) ;
#5794 =( GEOMETRIC_REPRESENTATION_CONTEXT ( 3 ) GLOBAL_UNCERTAINTY_ASSIGNED_CONTEXT ( ( #448 ) ) GLOBAL_UNIT_ASSIGNED_CONTEXT ( ( #1256, #10078, #13440 ) ) REPRESENTATION_CONTEXT ( 'NONE', 'WORKASPACE' ) );
#5795 = CARTESIAN_POINT ( 'NONE',  ( -124.9999999999999858, -115.2072594216369907, -7.500000000000000000 ) ) ;
#5796 = CIRCLE ( 'NONE', #14833, 2.649999999999992806 ) ;
#5797 = CARTESIAN_POINT ( 'NONE',  ( -1.261996585732579224, 4.276409079477648589, -7.062499998634407916 ) ) ;
#5798 = CARTESIAN_POINT ( 'NONE',  ( 1.206569728928466034, 7.963640680051485177, -0.4524126574264489831 ) ) ;
#5799 = DIRECTION ( 'NONE',  ( 3.111660235033397726E-14, 0.000000000000000000, 1.000000000000000000 ) ) ;
#5800 = CARTESIAN_POINT ( 'NONE',  ( 0.5093500532425063732, 4.799145180956616130, -7.124999998634407916 ) ) ;
#5801 = CARTESIAN_POINT ( 'NONE',  ( 5.809475019311125976, -13.00000000000000178, 1.500000000000000000 ) ) ;
#5802 = EDGE_CURVE ( 'NONE', #2074, #9076, #14799, .T. ) ;
#5803 = LINE ( 'NONE', #6720, #2539 ) ;
#5804 = EDGE_CURVE ( 'NONE', #7371, #79, #464, .T. ) ;
#5805 = CARTESIAN_POINT ( 'NONE',  ( 1.846868145590736310, -30.62500000136559208, 4.458734124999999437 ) ) ;
#5806 = ADVANCED_BREP_SHAPE_REPRESENTATION ( '', ( #14097, #3223 ), #7865 ) ;
#5807 = ORIENTED_EDGE ( 'NONE', *, *, #13824, .F. ) ;
#5808 = AXIS2_PLACEMENT_3D ( 'NONE', #9615, #10683, #9470 ) ;
#5809 = CARTESIAN_POINT ( 'NONE',  ( -1.846868145590734756, -24.12500000136559919, -4.458734124999999437 ) ) ;
#5810 = DIRECTION ( 'NONE',  ( 1.000000000000000000, -1.319090325525611458E-16, 0.000000000000000000 ) ) ;
#5811 = VERTEX_POINT ( 'NONE', #3752 ) ;
#5812 = VERTEX_POINT ( 'NONE', #6963 ) ;
#5814 = CARTESIAN_POINT ( 'NONE',  ( -54.99999999999999289, -25.00000000000000000, -17.50000000000000000 ) ) ;
#5813 = AXIS2_PLACEMENT_3D ( 'NONE', #8537, #14577, #3499 ) ;
#5815 = CARTESIAN_POINT ( 'NONE',  ( 4.458734124999999437, -29.50000000136559564, 1.846868145590737864 ) ) ;
#5816 = CARTESIAN_POINT ( 'NONE',  ( -5.000000000000002665, -1.404940523648820476E-14, -7.420263044861759028 ) ) ;
#5817 = ORIENTED_EDGE ( 'NONE', *, *, #5507, .T. ) ;
#5818 = CARTESIAN_POINT ( 'NONE',  ( -1.154700538379217711, -35.00000000000000000, -34.00000000000000000 ) ) ;
#5819 = VECTOR ( 'NONE', #6159, 1000.000000000000000 ) ;
#5820 = CARTESIAN_POINT ( 'NONE',  ( 2.071067811865505259, -22.18749999999999645, 4.999999999999970690 ) ) ;
#5821 = CARTESIAN_POINT ( 'NONE',  ( -45.00000000000000000, -34.99999999999999289, 13.35786437626904899 ) ) ;
#5822 = AXIS2_PLACEMENT_3D ( 'NONE', #662, #5666, #12997 ) ;
#5823 = CARTESIAN_POINT ( 'NONE',  ( 3.152801135295366208, -27.81250000136559564, 3.152801135295367985 ) ) ;
#5824 = FACE_OUTER_BOUND ( 'NONE', #507, .T. ) ;
#5825 = EDGE_CURVE ( 'NONE', #14592, #10616, #4595, .T. ) ;
#5826 = CARTESIAN_POINT ( 'NONE',  ( 4.391654732552941809, -2.390265405775130692, 0.000000000000000000 ) ) ;
#5827 = EDGE_CURVE ( 'NONE', #4880, #6007, #15949, .T. ) ;
#5828 = DIRECTION ( 'NONE',  ( -1.000000000000000000, 0.000000000000000000, 0.000000000000000000 ) ) ;
#5829 = ORIENTED_EDGE ( 'NONE', *, *, #12191, .T. ) ;
#5830 =( BOUNDED_SURFACE ( )  B_SPLINE_SURFACE ( 3, 2, ( 
 ( #13139, #10648, #8239 ),
 ( #15582, #4499, #11918 ),
 ( #9434, #14362, #7016 ),
 ( #5787, #15661, #13205 ),
 ( #4577, #9512, #12077 ),
 ( #10874, #944, #7176 ),
 ( #3369, #8316, #5872 ),
 ( #10805, #8389, #2221 ) ),
 .UNSPECIFIED., .F., .F., .F. ) 
 B_SPLINE_SURFACE_WITH_KNOTS ( ( 4, 2, 2, 4 ),
 ( 3, 3 ),
 ( 0.03861844051980969222, 0.04325213341840641185, 0.04556897986770477166, 0.04788582631700313147 ),
 ( 0.000000000000000000, 1.000000000000000000 ),
 .UNSPECIFIED. ) 
 GEOMETRIC_REPRESENTATION_ITEM ( )  RATIONAL_B_SPLINE_SURFACE ( (
 ( 1.000000000000000000, 0.8047781759831917903, 1.000000000000000000),
 ( 1.000000000000000000, 0.8123762462806505269, 1.000000000000000000),
 ( 1.000000000000000000, 0.8190659850614816495, 1.000000000000000000),
 ( 1.000000000000000000, 0.8191937571014599184, 1.000000000000000000),
 ( 1.000000000000000000, 0.8176092952781195411, 1.000000000000000000),
 ( 1.000000000000000000, 0.8122962088595742092, 1.000000000000000000),
 ( 1.000000000000000000, 0.8086311330828503952, 1.000000000000000000),
 ( 1.000000000000000000, 0.8047712282214323221, 1.000000000000000000) ) ) 
 REPRESENTATION_ITEM ( '' )  SURFACE ( )  );
#5831 = VECTOR ( 'NONE', #3754, 1000.000000000000000 ) ;
#5832 = SHAPE_REPRESENTATION_RELATIONSHIP ( 'NONE' , 'NONE' ,  #15130, #608 ) ;
#5833 = EDGE_LOOP ( 'NONE', ( #14308, #2703 ) ) ;
#5834 = CARTESIAN_POINT ( 'NONE',  ( 16.49999999999956657, -8.782289339527253835E-13, -6.000000000000000000 ) ) ;
#5835 = AXIS2_PLACEMENT_3D ( 'NONE', #14130, #11768, #13060 ) ;
#5836 = ORIENTED_EDGE ( 'NONE', *, *, #10295, .T. ) ;
#5837 = DIRECTION ( 'NONE',  ( 1.000000000000000000, 0.000000000000000000, 0.000000000000000000 ) ) ;
#5838 = AXIS2_PLACEMENT_3D ( 'NONE', #11406, #5269, #4054 ) ;
#5839 = CARTESIAN_POINT ( 'NONE',  ( -5.000000000000091482, -0.7223674278660691117, -3.396799362785969834 ) ) ;
#5840 = EDGE_CURVE ( 'NONE', #15429, #4698, #9378, .T. ) ;
#5841 = CARTESIAN_POINT ( 'NONE',  ( -2.131511515620587272, -3.916244202832140253, 1.312500001365592750 ) ) ;
#5842 = DIRECTION ( 'NONE',  ( 0.4999999999999919509, 0.000000000000000000, 0.8660254037844432595 ) ) ;
#5843 = AXIS2_PLACEMENT_3D ( 'NONE', #3276, #6764, #1818 ) ;
#5844 = ADVANCED_FACE ( 'NONE', ( #13075 ), #3226, .T. ) ;
#5845 = CARTESIAN_POINT ( 'NONE',  ( 3.916244202832140253, -2.131511515620588160, 0.3125000013655919728 ) ) ;
#5846 = CIRCLE ( 'NONE', #15412, 7.500000000000001776 ) ;
#5847 = CARTESIAN_POINT ( 'NONE',  ( 7.347880794884120722E-16, -11.00000000000000178, 6.000000000000000888 ) ) ;
#5848 = DIRECTION ( 'NONE',  ( 0.000000000000000000, 1.000000000000000000, 0.000000000000000000 ) ) ;
#5849 = EDGE_LOOP ( 'NONE', ( #942, #5299 ) ) ;
#5850 = CARTESIAN_POINT ( 'NONE',  ( -3.535533905932737309, -22.62500000000000000, -3.535533905932738197 ) ) ;
#5851 = PRESENTATION_STYLE_ASSIGNMENT (( #3268 ) ) ;
#5852 = ORIENTED_EDGE ( 'NONE', *, *, #2589, .F. ) ;
#5853 = DIRECTION ( 'NONE',  ( -0.000000000000000000, -0.000000000000000000, 1.000000000000000000 ) ) ;
#5854 = CIRCLE ( 'NONE', #14114, 2.000000000000000000 ) ;
#5855 = ORIENTED_EDGE ( 'NONE', *, *, #4282, .T. ) ;
#5856 = ORIENTED_EDGE ( 'NONE', *, *, #12929, .F. ) ;
#5857 = DIRECTION ( 'NONE',  ( 0.000000000000000000, 0.000000000000000000, 1.000000000000000000 ) ) ;
#5858 = CARTESIAN_POINT ( 'NONE',  ( -3.535533905932738641, -23.50000000273118772, 3.535533905932737309 ) ) ;
#5859 = AXIS2_PLACEMENT_3D ( 'NONE', #3964, #10118, #5432 ) ;
#5860 = PLANE ( 'NONE',  #15877 ) ;
#5861 = DIRECTION ( 'NONE',  ( 0.000000000000000000, 1.000000000000000000, 0.000000000000000000 ) ) ;
#5863 = CARTESIAN_POINT ( 'NONE',  ( -9.184850993605147944E-16, -24.37500000273118772, 5.000000000000000000 ) ) ;
#5862 = AXIS2_PLACEMENT_3D ( 'NONE', #9888, #7397, #7482 ) ;
#5864 = EDGE_CURVE ( 'NONE', #13141, #1955, #4330, .T. ) ;
#5865 = LINE ( 'NONE', #4726, #4607 ) ;
#5866 = FACE_OUTER_BOUND ( 'NONE', #14171, .T. ) ;
#5867 = FACE_OUTER_BOUND ( 'NONE', #9225, .T. ) ;
#5868 = FILL_AREA_STYLE ('',( #7171 ) ) ;
#5869 = CARTESIAN_POINT ( 'NONE',  ( -1.846868145590734756, -31.37500000136559564, -4.458734124999999437 ) ) ;
#5870 = CARTESIAN_POINT ( 'NONE',  ( -2.131511515620587272, -3.916244202832140253, 0.3125000013655919728 ) ) ;
#5871 = ORIENTED_EDGE ( 'NONE', *, *, #15347, .T. ) ;
#5872 = CARTESIAN_POINT ( 'NONE',  ( 0.6169862416621371137, 8.783631307151244627, -7.913704048099939214 ) ) ;
#5873 = EDGE_LOOP ( 'NONE', ( #1293, #545 ) ) ;
#5874 = ORIENTED_EDGE ( 'NONE', *, *, #3146, .T. ) ;
#5875 =( NAMED_UNIT ( * ) PLANE_ANGLE_UNIT ( ) SI_UNIT ( $, .RADIAN. ) );
#5876 = ORIENTED_EDGE ( 'NONE', *, *, #11616, .T. ) ;
#5877 = CARTESIAN_POINT ( 'NONE',  ( 1.846868145590735200, -26.50000000136559208, -4.458734125000000326 ) ) ;
#5878 = FACE_OUTER_BOUND ( 'NONE', #738, .T. ) ;
#5879 = CARTESIAN_POINT ( 'NONE',  ( 3.061616997868383141E-16, -25.87500000273118417, -5.000000000000000000 ) ) ;
#5880 = ADVANCED_FACE ( 'NONE', ( #10319 ), #11187, .F. ) ;
#5881 = AXIS2_PLACEMENT_3D ( 'NONE', #15072, #3914, #15158 ) ;
#5882 = DIRECTION ( 'NONE',  ( 0.000000000000000000, 0.000000000000000000, -1.000000000000000000 ) ) ;
#5883 = CARTESIAN_POINT ( 'NONE',  ( 5.000000000000002665, 3.306546357697854226E-16, 2.700000000000000622 ) ) ;
#5884 = CARTESIAN_POINT ( 'NONE',  ( -5.000000000000000000, -22.50000000000000000, -6.123233995736766282E-16 ) ) ;
#5885 = CARTESIAN_POINT ( 'NONE',  ( 2.390265326283148806, 4.391654775818395251, -2.875000000000002665 ) ) ;
#5886 = CARTESIAN_POINT ( 'NONE',  ( -2.071067811865492381, -21.43750000273118772, 4.999999999999985789 ) ) ;
#5887 = AXIS2_PLACEMENT_3D ( 'NONE', #10251, #151, #3773 ) ;
#5888 = CARTESIAN_POINT ( 'NONE',  ( 1.540890760463220044, -4.665335934641420934, -0.06581821247642098693 ) ) ;
#5889 = CARTESIAN_POINT ( 'NONE',  ( 1.846868145590735200, -31.25000000136559564, -4.458734125000000326 ) ) ;
#5890 = VECTOR ( 'NONE', #12290, 1000.000000000000000 ) ;
#5891 = ORIENTED_EDGE ( 'NONE', *, *, #5840, .F. ) ;
#5892 = DIRECTION ( 'NONE',  ( 0.000000000000000000, 0.000000000000000000, 1.000000000000000000 ) ) ;
#5893 = ORIENTED_EDGE ( 'NONE', *, *, #3480, .T. ) ;
#5894 = EDGE_LOOP ( 'NONE', ( #966, #373, #443 ) ) ;
#5895 = AXIS2_PLACEMENT_3D ( 'NONE', #8233, #8070, #13129 ) ;
#5896 = LINE ( 'NONE', #2476, #7983 ) ;
#5897 = AXIS2_PLACEMENT_3D ( 'NONE', #12664, #1604, #2651 ) ;
#5898 = CARTESIAN_POINT ( 'NONE',  ( -1.846868145590737420, -29.75000000136559564, 4.458734124999999437 ) ) ;
#5899 = CYLINDRICAL_SURFACE ( 'NONE', #4281, 4.250000000000000000 ) ;
#5900 = ORIENTED_EDGE ( 'NONE', *, *, #9965, .F. ) ;
#5901 = FACE_OUTER_BOUND ( 'NONE', #8336, .T. ) ;
#5902 = ADVANCED_FACE ( 'NONE', ( #455, #5377 ), #15245, .F. ) ;
#5903 = B_SPLINE_CURVE_WITH_KNOTS ( 'NONE', 3,
 ( #7131, #5914, #12356, #12186, #10838, #2408 ),
 .UNSPECIFIED., .F., .F.,
 ( 4, 2, 4 ),
 ( 0.000000000000000000, 0.0002095117440854740156, 0.0004190234881709480313 ),
 .UNSPECIFIED. ) ;
#5904 = VECTOR ( 'NONE', #15013, 1000.000000000000000 ) ;
#5905 = EDGE_CURVE ( 'NONE', #2868, #3779, #10233, .T. ) ;
#5906 = VECTOR ( 'NONE', #3893, 1000.000000000000000 ) ;
#5907 = DIRECTION ( 'NONE',  ( 0.000000000000000000, 0.000000000000000000, 1.000000000000000000 ) ) ;
#5908 = CARTESIAN_POINT ( 'NONE',  ( -115.0000000000000142, -10.00000000000000888, -7.500000000000000000 ) ) ;
#5909 = CYLINDRICAL_SURFACE ( 'NONE', #7051, 9.999999999999994671 ) ;
#5910 = AXIS2_PLACEMENT_3D ( 'NONE', #14748, #13275, #8618 ) ;
#5911 = CARTESIAN_POINT ( 'NONE',  ( -3.152801135295367096, -23.31250000136559564, -3.152801135295367541 ) ) ;
#5912 = TOROIDAL_SURFACE ( 'NONE', #1002, 2.700000000000001066, 0.2000000000000000111 ) ;
#5913 = CARTESIAN_POINT ( 'NONE',  ( -6.765421556309547668E-13, 40.00000000000000000, 64.84999999999931219 ) ) ;
#5914 = CARTESIAN_POINT ( 'NONE',  ( -6.259644161404862988E-16, -4.618802153517027165, -3.504271511726793076 ) ) ;
#5915 = CARTESIAN_POINT ( 'NONE',  ( -2.071067811865478170, -30.43750000273118417, 5.000000000000000000 ) ) ;
#5916 = CARTESIAN_POINT ( 'NONE',  ( 2.143131898507869826E-15, 40.00000000000000000, -67.50000000000000000 ) ) ;
#5917 = CIRCLE ( 'NONE', #2255, 5.000000000000000000 ) ;
#5918 = ORIENTED_EDGE ( 'NONE', *, *, #1684, .F. ) ;
#5919 = SHAPE_REPRESENTATION_RELATIONSHIP ( 'NONE' , 'NONE' ,  #9778, #6390 ) ;
#5920 = ORIENTED_EDGE ( 'NONE', *, *, #14818, .F. ) ;
#5921 = CARTESIAN_POINT ( 'NONE',  ( 0.000000000000000000, 20.00000000000000000, 0.000000000000000000 ) ) ;
#5922 = ORIENTED_EDGE ( 'NONE', *, *, #713, .F. ) ;
#5923 = ADVANCED_FACE ( 'NONE', ( #7571 ), #2935, .T. ) ;
#5924 = CARTESIAN_POINT ( 'NONE',  ( -3.535533905932737309, -26.62500000000000000, -3.535533905932738197 ) ) ;
#5925 = CARTESIAN_POINT ( 'NONE',  ( 1.415196051561583790, -4.795541693661363958, -4.124999997268816720 ) ) ;
#5926 = AXIS2_PLACEMENT_3D ( 'NONE', #6222, #76, #6685 ) ;
#5927 = CARTESIAN_POINT ( 'NONE',  ( 4.276409079477644148, 1.261996585732577891, -1.312499998634406140 ) ) ;
#5928 = DIRECTION ( 'NONE',  ( 6.123233995736766036E-17, 1.000000000000000000, 0.000000000000000000 ) ) ;
#5929 =( BOUNDED_CURVE ( )  B_SPLINE_CURVE ( 2, ( #5266, #6736, #9001, #13912, #2839, #1627, #589, #6565, #7790, #13984, #3093 ),
 .UNSPECIFIED., .F., .F. ) 
 B_SPLINE_CURVE_WITH_KNOTS ( ( 3, 2, 2, 2, 2, 3 ),
 ( 0.7545872658012773293, 0.7624999999999999556, 0.7750000000000000222, 0.7874999999999999778, 0.8000000000000000444, 0.8045872658012773737 ),
 .UNSPECIFIED. ) 
 CURVE ( )  GEOMETRIC_REPRESENTATION_ITEM ( )  RATIONAL_B_SPLINE_CURVE ( ( 0.9646335149384803742, 0.9518143178943441196, 1.000000000000000000, 0.9238795325112867385, 1.000000000000000000, 0.9238795325112867385, 1.000000000000000000, 0.9238795325112867385, 1.000000000000000000, 0.9720652146169423968, 0.9646335149384803742 ) ) 
 REPRESENTATION_ITEM ( '' )  );
#5930 = CARTESIAN_POINT ( 'NONE',  ( 2.131511515620586383, 3.916244202832140253, -0.4374999986344086933 ) ) ;
#5931 = DIRECTION ( 'NONE',  ( 0.000000000000000000, -1.000000000000000000, 0.000000000000000000 ) ) ;
#5932 = CARTESIAN_POINT ( 'NONE',  ( 4.211140560182196957, 2.431303136016536470, -3.745885042887433514 ) ) ;
#5933 = ORIENTED_EDGE ( 'NONE', *, *, #13519, .F. ) ;
#5934 = FACE_OUTER_BOUND ( 'NONE', #1095, .T. ) ;
#5935 = EDGE_LOOP ( 'NONE', ( #12559, #8528 ) ) ;
#5936 = DIRECTION ( 'NONE',  ( -0.000000000000000000, 1.000000000000000000, -0.000000000000000000 ) ) ;
#5937 = VERTEX_POINT ( 'NONE', #5143 ) ;
#5938 = ORIENTED_EDGE ( 'NONE', *, *, #13620, .F. ) ;
#5939 = CARTESIAN_POINT ( 'NONE',  ( 2.131511515620586383, 3.916244202832140253, -1.437499998634406140 ) ) ;
#5940 = EDGE_CURVE ( 'NONE', #5482, #10782, #7186, .T. ) ;
#5941 = EDGE_CURVE ( 'NONE', #6708, #3920, #1747, .T. ) ;
#5942 = ADVANCED_FACE ( 'NONE', ( #15001 ), #13606, .T. ) ;
#5943 = EDGE_CURVE ( 'NONE', #10287, #434, #7175, .T. ) ;
#5944 =( NAMED_UNIT ( * ) PLANE_ANGLE_UNIT ( ) SI_UNIT ( $, .RADIAN. ) );
#5945 = CARTESIAN_POINT ( 'NONE',  ( -7.894787914004613327, 0.7647108141804107584, -7.591390474663421095 ) ) ;
#5946 = DIRECTION ( 'NONE',  ( 0.8660254037844405950, -0.4999999999999965028, -0.000000000000000000 ) ) ;
#5947 = DIRECTION ( 'NONE',  ( -0.000000000000000000, 1.000000000000000000, -0.000000000000000000 ) ) ;
#5948 = CARTESIAN_POINT ( 'NONE',  ( -0.5711823568785978633, -5.381735091635035495, -0.1874999972688185246 ) ) ;
#5949 = CARTESIAN_POINT ( 'NONE',  ( 2.143131898507869826E-15, 37.00000000000000000, -70.15000000000000568 ) ) ;
#5950 = PLANE ( 'NONE',  #231 ) ;
#5951 = CARTESIAN_POINT ( 'NONE',  ( -4.458734125000000326, -30.12500000136559564, 1.846868145590734089 ) ) ;
#5952 = CARTESIAN_POINT ( 'NONE',  ( -1.261996585732579224, 4.276409079477648589, -4.062499998634405252 ) ) ;
#5953 = ORIENTED_EDGE ( 'NONE', *, *, #15289, .F. ) ;
#5954 = FACE_OUTER_BOUND ( 'NONE', #8604, .T. ) ;
#5955 = VERTEX_POINT ( 'NONE', #4075 ) ;
#5956 = ORIENTED_EDGE ( 'NONE', *, *, #10861, .T. ) ;
#5957 =( LENGTH_UNIT ( ) NAMED_UNIT ( * ) SI_UNIT ( .MILLI., .METRE. ) );
#5958 = EDGE_LOOP ( 'NONE', ( #10585, #7409, #11335, #5236 ) ) ;
#5959 = LINE ( 'NONE', #15822, #11281 ) ;
#5960 = CARTESIAN_POINT ( 'NONE',  ( -21.01110699893041556, 0.000000000000000000, -36.39230484541334221 ) ) ;
#5961 = ADVANCED_FACE ( 'NONE', ( #5052 ), #7814, .T. ) ;
#5962 = FACE_OUTER_BOUND ( 'NONE', #14063, .T. ) ;
#5963 = B_SPLINE_CURVE_WITH_KNOTS ( 'NONE', 3,
 ( #14478, #13094, #6069, #2032, #4536, #3473 ),
 .UNSPECIFIED., .F., .F.,
 ( 4, 2, 4 ),
 ( 0.002452478801916361129, 0.003676905084148001344, 0.004901331366379641126 ),
 .UNSPECIFIED. ) ;
#5964 = PLANE ( 'NONE',  #12294 ) ;
#5965 = CARTESIAN_POINT ( 'NONE',  ( -124.9999999999999858, -115.2072594216369907, 7.500000000000001776 ) ) ;
#5966 = CARTESIAN_POINT ( 'NONE',  ( 0.2500000000000002220, 0.000000000000000000, 0.000000000000000000 ) ) ;
#5967 = CARTESIAN_POINT ( 'NONE',  ( -5.381735091635034607, 0.5711823568785950878, -0.5624999999999995559 ) ) ;
#5968 = CARTESIAN_POINT ( 'NONE',  ( 0.2500000000000002220, 0.000000000000000000, 0.000000000000000000 ) ) ;
#5969 = LINE ( 'NONE', #3691, #7717 ) ;
#5970 = CARTESIAN_POINT ( 'NONE',  ( -3.152801135295367985, -29.81250000136559208, 3.152801135295367096 ) ) ;
#5971 = CARTESIAN_POINT ( 'NONE',  ( 0.5093500532425063732, 4.799145180956616130, 0.6250000013655918618 ) ) ;
#5972 = VERTEX_POINT ( 'NONE', #9029 ) ;
#5973 = CARTESIAN_POINT ( 'NONE',  ( 7.848314987057847247, -4.129027267381571775, -7.493854785173811983 ) ) ;
#5974 = ORIENTED_EDGE ( 'NONE', *, *, #3382, .F. ) ;
#5975 = ORIENTED_EDGE ( 'NONE', *, *, #11336, .F. ) ;
#5976 = CARTESIAN_POINT ( 'NONE',  ( -7.894955577759749765, 1.603085139987818764, -7.593799241562204649 ) ) ;
#5977 = CARTESIAN_POINT ( 'NONE',  ( -3.152801135295367096, -27.06250000136559564, -3.152801135295367541 ) ) ;
#5978 = DIRECTION ( 'NONE',  ( -0.000000000000000000, -1.000000000000000000, -0.000000000000000000 ) ) ;
#5979 = ORIENTED_EDGE ( 'NONE', *, *, #1610, .T. ) ;
#5980 = DIRECTION ( 'NONE',  ( 0.000000000000000000, 0.000000000000000000, 1.000000000000000000 ) ) ;
#5981 = CARTESIAN_POINT ( 'NONE',  ( -3.750000000000004885, 6.495190528383289141, 0.000000000000000000 ) ) ;
#5982 = CARTESIAN_POINT ( 'NONE',  ( 57.73502691896258199, 0.000000000000000000, 2.081668171172168513E-14 ) ) ;
#5983 = CARTESIAN_POINT ( 'NONE',  ( -5.725490332117410652, -3.000000000000000000, 9.916840153471811803 ) ) ;
#5984 = CARTESIAN_POINT ( 'NONE',  ( 1.846868145590735200, -23.50000000136559564, -4.458734125000000326 ) ) ;
#5985 = DIRECTION ( 'NONE',  ( 0.000000000000000000, 1.000000000000000000, -0.000000000000000000 ) ) ;
#5986 = CARTESIAN_POINT ( 'NONE',  ( 3.401574460001763445, -4.209348295687703079, -1.062499997268813612 ) ) ;
#5987 = CARTESIAN_POINT ( 'NONE',  ( -5.000000000000000888, -30.56250000273118417, 2.071067811865474617 ) ) ;
#5988 = CARTESIAN_POINT ( 'NONE',  ( -5.000000000000003553, -1.404940523648820476E-14, -6.545263047592945860 ) ) ;
#5989 = DIRECTION ( 'NONE',  ( 0.000000000000000000, 0.000000000000000000, 1.000000000000000000 ) ) ;
#5990 = EDGE_CURVE ( 'NONE', #4542, #10705, #3809, .T. ) ;
#5991 = AXIS2_PLACEMENT_3D ( 'NONE', #8380, #3358, #15808 ) ;
#5993 = EDGE_CURVE ( 'NONE', #8265, #15092, #13093, .T. ) ;
#5992 = ORIENTED_EDGE ( 'NONE', *, *, #4009, .F. ) ;
#5994 = EDGE_LOOP ( 'NONE', ( #9149, #1374 ) ) ;
#5995 = DIRECTION ( 'NONE',  ( 0.000000000000000000, 0.000000000000000000, 1.000000000000000000 ) ) ;
#5996 = VERTEX_POINT ( 'NONE', #6353 ) ;
#5997 = LINE ( 'NONE', #12126, #10460 ) ;
#5998 = AXIS2_PLACEMENT_3D ( 'NONE', #11015, #7070, #997 ) ;
#5999 = CARTESIAN_POINT ( 'NONE',  ( -5.725490332106780933, -3.000000000000000000, -9.916840153467775920 ) ) ;
#6000 = CIRCLE ( 'NONE', #13731, 30.00000000000000711 ) ;
#6001 = CARTESIAN_POINT ( 'NONE',  ( -2.131511515620587272, -3.916244202832140253, 0.3125000013655919728 ) ) ;
#6002 = DIRECTION ( 'NONE',  ( 6.123233995736766036E-17, 1.000000000000000000, 0.000000000000000000 ) ) ;
#6003 = CARTESIAN_POINT ( 'NONE',  ( 2.131511515620586383, 3.916244202832140253, -2.437499998634407028 ) ) ;
#6004 = CYLINDRICAL_SURFACE ( 'NONE', #13063, 2.500000000000000444 ) ;
#6005 = ADVANCED_FACE ( 'NONE', ( #8859 ), #6589, .T. ) ;
#6006 = EDGE_CURVE ( 'NONE', #15603, #12752, #12469, .T. ) ;
#6007 = VERTEX_POINT ( 'NONE', #2698 ) ;
#6008 = CARTESIAN_POINT ( 'NONE',  ( 0.000000000000000000, 0.000000000000000000, 0.000000000000000000 ) ) ;
#6009 = PRODUCT_DEFINITION ( 'UNKNOWN', '', #6905, #6432 ) ;
#6010 = ORIENTED_EDGE ( 'NONE', *, *, #11388, .T. ) ;
#6011 = DIRECTION ( 'NONE',  ( 0.000000000000000000, 1.000000000000000000, 0.000000000000000000 ) ) ;
#6012 = ORIENTED_EDGE ( 'NONE', *, *, #3346, .F. ) ;
#6013 = VECTOR ( 'NONE', #13724, 1000.000000000000000 ) ;
#6014 = ORIENTED_EDGE ( 'NONE', *, *, #2929, .F. ) ;
#6015 = CARTESIAN_POINT ( 'NONE',  ( 1.261996585732578113, -4.276409079477644148, -4.812499998634405252 ) ) ;
#6016 = AXIS2_PLACEMENT_3D ( 'NONE', #7927, #15106, #10184 ) ;
#6017 = DIRECTION ( 'NONE',  ( 0.000000000000000000, 0.000000000000000000, 1.000000000000000000 ) ) ;
#6018 =( BOUNDED_CURVE ( )  B_SPLINE_CURVE ( 2, ( #6822, #11581, #533, #1960, #1642, #6749, #15239, #10312, #14000, #7881, #4147 ),
 .UNSPECIFIED., .F., .F. ) 
 B_SPLINE_CURVE_WITH_KNOTS ( ( 3, 2, 2, 2, 2, 3 ),
 ( 0.9045872658012773515, 0.9124999999999999778, 0.9250000000000000444, 0.9375000000000000000, 0.9499999999999999556, 0.9545872658012772849 ),
 .UNSPECIFIED. ) 
 CURVE ( )  GEOMETRIC_REPRESENTATION_ITEM ( )  RATIONAL_B_SPLINE_CURVE ( ( 0.9646335149384803742, 0.9518143178943441196, 1.000000000000000000, 0.9238795325112867385, 1.000000000000000000, 0.9238795325112867385, 1.000000000000000000, 0.9238795325112867385, 1.000000000000000000, 0.9720652146169428409, 0.9646335149384808183 ) ) 
 REPRESENTATION_ITEM ( '' )  );
#6019 = CARTESIAN_POINT ( 'NONE',  ( 2.131511515620586383, 3.916244202832140253, -8.187499998634407916 ) ) ;
#6020 = AXIS2_PLACEMENT_3D ( 'NONE', #10249, #4093, #5396 ) ;
#6021 = DIRECTION ( 'NONE',  ( 0.000000000000000000, -0.4999999999999993894, 0.8660254037844389297 ) ) ;
#6022 = CARTESIAN_POINT ( 'NONE',  ( 24.26932219902320043, 37.00000000000000000, 5.999999999999992895 ) ) ;
#6023 = LINE ( 'NONE', #9575, #10038 ) ;
#6024 = CARTESIAN_POINT ( 'NONE',  ( -8.673617379884035472E-16, -9.147862274876560562, -8.047472243342939535 ) ) ;
#6025 = EDGE_CURVE ( 'NONE', #13521, #2121, #7656, .T. ) ;
#6026 = PRODUCT_DEFINITION ( 'UNKNOWN', '', #3014, #2690 ) ;
#6027 =( NAMED_UNIT ( * ) SI_UNIT ( $, .STERADIAN. ) SOLID_ANGLE_UNIT ( ) );
#6028 = CARTESIAN_POINT ( 'NONE',  ( 4.458734124999999437, -25.62500000136559564, -1.846868145590734978 ) ) ;
#6029 = ADVANCED_FACE ( 'NONE', ( #13854 ), #9263, .F. ) ;
#6030 = CARTESIAN_POINT ( 'NONE',  ( -4.799145180956616130, 0.5093500532425063732, -3.874999998634404363 ) ) ;
#6031 = CARTESIAN_POINT ( 'NONE',  ( 0.000000000000000000, 20.00000000000000000, 0.000000000000000000 ) ) ;
#6032 = ORIENTED_EDGE ( 'NONE', *, *, #1261, .F. ) ;
#6033 = ORIENTED_EDGE ( 'NONE', *, *, #2677, .F. ) ;
#6034 = FILL_AREA_STYLE_COLOUR ( '', #10947 ) ;
#6035 = VERTEX_POINT ( 'NONE', #5617 ) ;
#6036 = PRODUCT ( 'connector', 'connector', '', ( #7465 ) ) ;
#6037 = CARTESIAN_POINT ( 'NONE',  ( 1.846868145590736310, -24.87500000136559919, 4.458734124999999437 ) ) ;
#6038 = CARTESIAN_POINT ( 'NONE',  ( 0.000000000000000000, 40.00000000000000000, 75.00000000000001421 ) ) ;
#6039 = CARTESIAN_POINT ( 'NONE',  ( 5.000000000000000000, -30.12500000273118417, 0.000000000000000000 ) ) ;
#6040 = LINE ( 'NONE', #12240, #15671 ) ;
#6041 = FACE_BOUND ( 'NONE', #8449, .T. ) ;
#6042 = CARTESIAN_POINT ( 'NONE',  ( -5.000000000000000000, -23.50000000000000000, -6.123233995736766282E-16 ) ) ;
#6043 = CARTESIAN_POINT ( 'NONE',  ( 4.391654775818395251, -2.390265326283149694, -3.125000000000002665 ) ) ;
#6044 = CARTESIAN_POINT ( 'NONE',  ( 0.5711823568785988625, 5.381735091635026613, -3.812499999999998668 ) ) ;
#6045 = CARTESIAN_POINT ( 'NONE',  ( -5.000000000000000888, -27.43750000000000355, 2.071067811865474617 ) ) ;
#6046 = CARTESIAN_POINT ( 'NONE',  ( 4.458734125000000326, -27.37500000136559564, -1.846868145590734978 ) ) ;
#6047 = EDGE_CURVE ( 'NONE', #13808, #739, #4848, .T. ) ;
#6048 = CARTESIAN_POINT ( 'NONE',  ( -4.276409079477644148, -1.261996585732578335, -2.062499998634406584 ) ) ;
#6049 = ORIENTED_EDGE ( 'NONE', *, *, #1623, .T. ) ;
#6050 = CARTESIAN_POINT ( 'NONE',  ( 7.970070017554209407, -4.546953124339768060, -8.057670357645360326 ) ) ;
#6051 = ORIENTED_EDGE ( 'NONE', *, *, #1383, .F. ) ;
#6052 = ORIENTED_EDGE ( 'NONE', *, *, #13497, .T. ) ;
#6053 = CARTESIAN_POINT ( 'NONE',  ( -7.500000000000003553, -1.572902445675431471, -7.069816568113128419 ) ) ;
#6054 = AXIS2_PLACEMENT_3D ( 'NONE', #7413, #6204, #12317 ) ;
#6055 = CARTESIAN_POINT ( 'NONE',  ( -8.190561711645485556E-16, -25.68750000136559564, 4.458734124999999437 ) ) ;
#6056 = DIRECTION ( 'NONE',  ( 0.000000000000000000, 0.000000000000000000, 1.000000000000000000 ) ) ;
#6057 = VECTOR ( 'NONE', #664, 1000.000000000000227 ) ;
#6058 = VERTEX_POINT ( 'NONE', #5457 ) ;
#6059 = CARTESIAN_POINT ( 'NONE',  ( -6.765421556309547668E-13, 50.00000000000000000, 67.49999999999930367 ) ) ;
#6060 = CARTESIAN_POINT ( 'NONE',  ( -9.184850993605147944E-16, -22.25000000000000000, 4.999999999999999112 ) ) ;
#6061 = CARTESIAN_POINT ( 'NONE',  ( 4.024499207728657879, 2.323545700935571556, -3.572172305156506411 ) ) ;
#6062 = DIRECTION ( 'NONE',  ( 0.000000000000000000, 0.000000000000000000, -1.000000000000000000 ) ) ;
#6063 = CARTESIAN_POINT ( 'NONE',  ( -8.190561711645485556E-16, -23.93750000136559564, 4.458734124999999437 ) ) ;
#6064 = LINE ( 'NONE', #8580, #12423 ) ;
#6065 = CARTESIAN_POINT ( 'NONE',  ( 3.333333333333332593, 2.694301256218250007, -3.300726591567078483 ) ) ;
#6066 = CARTESIAN_POINT ( 'NONE',  ( 5.000000000000000888, -28.06250000273118772, -2.071067811865475505 ) ) ;
#6067 = VECTOR ( 'NONE', #8141, 1000.000000000000000 ) ;
#6068 = CARTESIAN_POINT ( 'NONE',  ( -5.000000000000004441, -1.011557177027151181E-15, -6.420263044861759028 ) ) ;
#6069 = CARTESIAN_POINT ( 'NONE',  ( 4.198928548860774157, -0.8158838809860124996, -3.526471437616918170 ) ) ;
#6070 = CARTESIAN_POINT ( 'NONE',  ( 5.560781378645573980, 6.809993116116507654E-16, -4.000000000000000000 ) ) ;
#6071 = VERTEX_POINT ( 'NONE', #3266 ) ;
#6072 = ORIENTED_EDGE ( 'NONE', *, *, #6505, .F. ) ;
#6073 = CARTESIAN_POINT ( 'NONE',  ( 0.000000000000000000, -11.00000000000000178, 5.000000000000000000 ) ) ;
#6074 = B_SPLINE_CURVE_WITH_KNOTS ( 'NONE', 3,
 ( #11773, #5651, #13066, #10594, #15518, #6953, #11855, #803, #14373, #7504, #2232, #15907, #6126, #15827, #4745, #65 ),
 .UNSPECIFIED., .F., .F.,
 ( 4, 2, 2, 2, 2, 2, 2, 4 ),
 ( 1.371419323662773723E-18, 0.0003988081628697417893, 0.0007976163257394822776, 0.001196424488609222712, 0.001595232651478961953, 0.001994040814348701195, 0.002392848977218440219, 0.003190465302957923906 ),
 .UNSPECIFIED. ) ;
#6075 = VECTOR ( 'NONE', #11865, 1000.000000000000000 ) ;
#6076 = EDGE_LOOP ( 'NONE', ( #695, #654, #9307, #12793 ) ) ;
#6077 = DIRECTION ( 'NONE',  ( 0.000000000000000000, 0.000000000000000000, -1.000000000000000000 ) ) ;
#6078 = AXIS2_PLACEMENT_3D ( 'NONE', #4804, #11028, #14502 ) ;
#6079 = EDGE_CURVE ( 'NONE', #10036, #7945, #690, .T. ) ;
#6080 = CARTESIAN_POINT ( 'NONE',  ( -2.886751345948099789, 0.000000000000000000, -35.00000000000000000 ) ) ;
#6081 = CARTESIAN_POINT ( 'NONE',  ( -4.276409079477644148, -1.261996585732578335, 1.187500001365592750 ) ) ;
#6082 = CARTESIAN_POINT ( 'NONE',  ( 67.49999999999933209, 55.00000000000000711, 2.081668171172168513E-14 ) ) ;
#6083 = AXIS2_PLACEMENT_3D ( 'NONE', #417, #7854, #7782 ) ;
#6084 = CARTESIAN_POINT ( 'NONE',  ( 4.276409079477644148, 1.261996585732577891, 0.4375000013655920839 ) ) ;
#6085 = PRESENTATION_STYLE_ASSIGNMENT (( #32 ) ) ;
#6086 = AXIS2_PLACEMENT_3D ( 'NONE', #271, #2833, #185 ) ;
#6087 = LINE ( 'NONE', #8369, #4859 ) ;
#6088 = AXIS2_PLACEMENT_3D ( 'NONE', #14470, #15536, #15372 ) ;
#6089 =( REPRESENTATION_RELATIONSHIP ('NONE','NONE', #4176, #10906 ) REPRESENTATION_RELATIONSHIP_WITH_TRANSFORMATION ( #116 )SHAPE_REPRESENTATION_RELATIONSHIP( ) );
#6090 = VERTEX_POINT ( 'NONE', #1729 ) ;
#6091 = DIRECTION ( 'NONE',  ( 0.000000000000000000, 0.000000000000000000, -1.000000000000000000 ) ) ;
#6092 = CARTESIAN_POINT ( 'NONE',  ( 2.500000000000000000, 2.357898499370433054, -1.951563910473907981E-15 ) ) ;
#6093 = EDGE_CURVE ( 'NONE', #4594, #10386, #10771, .T. ) ;
#6094 = ORIENTED_EDGE ( 'NONE', *, *, #6240, .T. ) ;
#6095 = CARTESIAN_POINT ( 'NONE',  ( -0.5093500532425060401, -4.799145180956616130, -2.874999998634407472 ) ) ;
#6096 = ADVANCED_FACE ( 'NONE', ( #14259 ), #6680, .F. ) ;
#6097 = EDGE_CURVE ( 'NONE', #3419, #10619, #9180, .T. ) ;
#6098 = VECTOR ( 'NONE', #2967, 1000.000000000000000 ) ;
#6099 = CARTESIAN_POINT ( 'NONE',  ( -5.000000000000000000, -29.50000000000000355, -6.123233995736766282E-16 ) ) ;
#6100 = AXIS2_PLACEMENT_3D ( 'NONE', #2361, #4798, #8602 ) ;
#6101 = FACE_OUTER_BOUND ( 'NONE', #3099, .T. ) ;
#6102 = CYLINDRICAL_SURFACE ( 'NONE', #15029, 2.649999999999992806 ) ;
#6103 = UNCERTAINTY_MEASURE_WITH_UNIT (LENGTH_MEASURE( 1.000000000000000082E-05 ), #10053, 'distance_accuracy_value', 'NONE');
#6104 = CARTESIAN_POINT ( 'NONE',  ( -3.535533905932738641, -29.50000000273118417, 3.535533905932737309 ) ) ;
#6105 = CARTESIAN_POINT ( 'NONE',  ( 4.795541693661363958, 1.415196051561583790, -1.874999997268814944 ) ) ;
#6106 = FILL_AREA_STYLE_COLOUR ( '', #11575 ) ;
#6107 = VECTOR ( 'NONE', #12527, 1000.000000000000000 ) ;
#6108 = PRESENTATION_STYLE_ASSIGNMENT (( #10870 ) ) ;
#6109 = CARTESIAN_POINT ( 'NONE',  ( 3.152801135295367541, -24.56250000136559564, -3.152801135295367541 ) ) ;
#6110 = CARTESIAN_POINT ( 'NONE',  ( -4.458734124999999437, -23.93750000136559564, -5.460374474430324690E-16 ) ) ;
#6111 = CARTESIAN_POINT ( 'NONE',  ( -3.916244202832140253, 2.131511515620587272, -3.937499998634404808 ) ) ;
#6112 = CARTESIAN_POINT ( 'NONE',  ( -3.750000000000004885, 6.495190528383289141, 0.000000000000000000 ) ) ;
#6113 = ORIENTED_EDGE ( 'NONE', *, *, #11650, .T. ) ;
#6114 = EDGE_LOOP ( 'NONE', ( #10895, #8412 ) ) ;
#6115 = CARTESIAN_POINT ( 'NONE',  ( 3.152801135295366208, -24.81250000136559564, 3.152801135295367985 ) ) ;
#6116 = VECTOR ( 'NONE', #6449, 1000.000000000000000 ) ;
#6117 = CARTESIAN_POINT ( 'NONE',  ( 0.000000000000000000, 0.000000000000000000, 0.000000000000000000 ) ) ;
#6118 = ORIENTED_EDGE ( 'NONE', *, *, #9075, .F. ) ;
#6119 = CARTESIAN_POINT ( 'NONE',  ( 4.458734124999999437, -24.75000000136559564, 1.846868145590737864 ) ) ;
#6120 = CARTESIAN_POINT ( 'NONE',  ( -5.000000000000000888, -23.56250000273118772, 2.071067811865474617 ) ) ;
#6121 = CARTESIAN_POINT ( 'NONE',  ( 3.061616997868383141E-16, -27.87500000273118772, -5.000000000000000000 ) ) ;
#6122 = EDGE_CURVE ( 'NONE', #11587, #717, #10282, .T. ) ;
#6123 = AXIS2_PLACEMENT_3D ( 'NONE', #3122, #6843, #14273 ) ;
#6124 = ADVANCED_FACE ( 'NONE', ( #540 ), #10387, .T. ) ;
#6125 = FACE_OUTER_BOUND ( 'NONE', #478, .T. ) ;
#6126 = CARTESIAN_POINT ( 'NONE',  ( 4.686367213310268731, -4.097106062772740920, 48.53802711916877399 ) ) ;
#6127 = DIRECTION ( 'NONE',  ( 0.000000000000000000, 0.000000000000000000, 1.000000000000000000 ) ) ;
#6128 = CIRCLE ( 'NONE', #6401, 2.649999999999999467 ) ;
#6129 = CARTESIAN_POINT ( 'NONE',  ( 3.401574460001763001, -4.209348295687703967, -1.187500000000001998 ) ) ;
#6130 = CARTESIAN_POINT ( 'NONE',  ( -3.401574460001765221, 4.209348295687701302, -3.687500000000000444 ) ) ;
#6131 = CARTESIAN_POINT ( 'NONE',  ( 4.257627111623017768, -2.623238587170121594, -0.004444259227768714363 ) ) ;
#6132 = CARTESIAN_POINT ( 'NONE',  ( -3.152801135295367096, -27.06250000136559564, -3.152801135295367541 ) ) ;
#6133 = CARTESIAN_POINT ( 'NONE',  ( 1.261996585732578113, -4.276409079477644148, -2.812499998634407472 ) ) ;
#6134 = ORIENTED_EDGE ( 'NONE', *, *, #13573, .T. ) ;
#6135 = DIRECTION ( 'NONE',  ( 1.000000000000000000, 0.000000000000000000, 0.000000000000000000 ) ) ;
#6136 = ORIENTED_EDGE ( 'NONE', *, *, #3940, .F. ) ;
#6137 = CIRCLE ( 'NONE', #967, 4.250000000000000000 ) ;
#6138 = EDGE_LOOP ( 'NONE', ( #13352, #7956, #4521 ) ) ;
#6139 = CARTESIAN_POINT ( 'NONE',  ( -99.99999999999998579, -100.7735026918962831, -17.50000000000000000 ) ) ;
#6140 = CARTESIAN_POINT ( 'NONE',  ( 1.846868145590736310, -26.62500000136559564, 4.458734124999999437 ) ) ;
#6141 = CARTESIAN_POINT ( 'NONE',  ( 16.49999999999956657, -8.782289339527253835E-13, -4.500000000000000000 ) ) ;
#6142 = ORIENTED_EDGE ( 'NONE', *, *, #6676, .T. ) ;
#6143 = CIRCLE ( 'NONE', #12568, 2.499999999999998668 ) ;
#6144 = CIRCLE ( 'NONE', #10283, 25.00000000000000000 ) ;
#6145 = PLANE ( 'NONE',  #926 ) ;
#6146 = EDGE_CURVE ( 'NONE', #10453, #12212, #11895, .T. ) ;
#6147 = EDGE_CURVE ( 'NONE', #7997, #13263, #14660, .T. ) ;
#6149 = CIRCLE ( 'NONE', #1225, 2.649999999999999467 ) ;
#6148 = DIRECTION ( 'NONE',  ( 0.000000000000000000, 0.000000000000000000, -1.000000000000000000 ) ) ;
#6150 = CARTESIAN_POINT ( 'NONE',  ( -158.0560796608385488, -84.57531754730580076, -17.50000000000000000 ) ) ;
#6151 = FACE_BOUND ( 'NONE', #14405, .T. ) ;
#6152 = CARTESIAN_POINT ( 'NONE',  ( -3.152801135295367985, -24.06250000136559564, 3.152801135295367096 ) ) ;
#6153 = DIRECTION ( 'NONE',  ( -1.000000000000000000, 0.000000000000000000, -0.000000000000000000 ) ) ;
#6154 = FACE_OUTER_BOUND ( 'NONE', #7747, .T. ) ;
#6155 = CARTESIAN_POINT ( 'NONE',  ( 5.000000000000000000, -30.18750000273118772, 2.071067811865478614 ) ) ;
#6156 = CARTESIAN_POINT ( 'NONE',  ( -124.9999999999999716, -10.00000000000001066, 7.500000000000001776 ) ) ;
#6157 = AXIS2_PLACEMENT_3D ( 'NONE', #10834, #5002, #13551 ) ;
#6158 = CARTESIAN_POINT ( 'NONE',  ( 4.458734124999997661, -29.50000000136559564, 1.846868145590737864 ) ) ;
#6159 = DIRECTION ( 'NONE',  ( -1.000000000000000000, -0.000000000000000000, -0.000000000000000000 ) ) ;
#6160 = ORIENTED_EDGE ( 'NONE', *, *, #205, .F. ) ;
#6161 = PRESENTATION_STYLE_ASSIGNMENT (( #4778 ) ) ;
#6162 = EDGE_LOOP ( 'NONE', ( #11254, #13347, #14303 ) ) ;
#6163 = CARTESIAN_POINT ( 'NONE',  ( 2.000000000000008882, 3.464101615137749945, 0.000000000000000000 ) ) ;
#6164 = CIRCLE ( 'NONE', #5652, 30.00000000000000711 ) ;
#6165 = VERTEX_POINT ( 'NONE', #15320 ) ;
#6166 = PLANE ( 'NONE',  #8962 ) ;
#6167 = ADVANCED_FACE ( 'NONE', ( #9411 ), #5765, .T. ) ;
#6168 = CIRCLE ( 'NONE', #13634, 60.00000000000000000 ) ;
#6169 = DIRECTION ( 'NONE',  ( 0.000000000000000000, 0.000000000000000000, 1.000000000000000000 ) ) ;
#6170 = CARTESIAN_POINT ( 'NONE',  ( -3.753672977998669946, -3.033343224707661712, -2.749999998634409248 ) ) ;
#6171 = AXIS2_PLACEMENT_3D ( 'NONE', #2136, #15653, #15740 ) ;
#6172 = PRODUCT_CONTEXT ( 'NONE', #4001, 'mechanical' ) ;
#6173 = AXIS2_PLACEMENT_3D ( 'NONE', #14136, #15193, #11771 ) ;
#6174 = CARTESIAN_POINT ( 'NONE',  ( -2.131511515620587272, -3.916244202832140253, -4.937499998634406140 ) ) ;
#6175 = DIRECTION ( 'NONE',  ( -0.000000000000000000, -1.000000000000000000, -0.000000000000000000 ) ) ;
#6176 = CARTESIAN_POINT ( 'NONE',  ( 30.02221399786052913, 0.000000000000000000, 16.00000000000001066 ) ) ;
#6177 = LINE ( 'NONE', #7152, #10031 ) ;
#6178 = DIRECTION ( 'NONE',  ( 1.000000000000000000, 0.000000000000000000, 0.000000000000000000 ) ) ;
#6179 = EDGE_CURVE ( 'NONE', #9532, #2616, #12100, .T. ) ;
#6180 = ORIENTED_EDGE ( 'NONE', *, *, #979, .T. ) ;
#6181 = CARTESIAN_POINT ( 'NONE',  ( 1.415196051561583790, -4.795541693661363958, -1.250000000000001110 ) ) ;
#6182 = ORIENTED_EDGE ( 'NONE', *, *, #14524, .F. ) ;
#6183 = ORIENTED_EDGE ( 'NONE', *, *, #10103, .T. ) ;
#6184 = CONTEXT_DEPENDENT_SHAPE_REPRESENTATION ( #4951, #15014 ) ;
#6185 = CARTESIAN_POINT ( 'NONE',  ( -4.799145180956616130, 0.5093500532425063732, -4.124999998634405252 ) ) ;
#6186 = DIRECTION ( 'NONE',  ( 0.000000000000000000, 0.000000000000000000, 1.000000000000000000 ) ) ;
#6187 = AXIS2_PLACEMENT_3D ( 'NONE', #5769, #5853, #8218 ) ;
#6188 = DIRECTION ( 'NONE',  ( 0.000000000000000000, 1.000000000000000000, 0.000000000000000000 ) ) ;
#6189 = DIRECTION ( 'NONE',  ( -1.000000000000000000, 0.000000000000000000, 0.000000000000000000 ) ) ;
#6190 = CARTESIAN_POINT ( 'NONE',  ( 3.401574460001763445, -4.209348295687703079, -2.187500000000002665 ) ) ;
#6191 = CYLINDRICAL_SURFACE ( 'NONE', #5129, 2.500000000000000444 ) ;
#6192 = EDGE_CURVE ( 'NONE', #15071, #1633, #10543, .T. ) ;
#6193 = CARTESIAN_POINT ( 'NONE',  ( -4.336808689942017736E-16, -8.660254037844399733, -7.422398894150038728 ) ) ;
#6194 = CARTESIAN_POINT ( 'NONE',  ( -1.154700538379255903, 0.000000000000000000, 34.00000000000000711 ) ) ;
#6195 = FACE_OUTER_BOUND ( 'NONE', #15435, .T. ) ;
#6196 = CARTESIAN_POINT ( 'NONE',  ( -1.846868145590737420, -27.00000000136559564, 4.458734124999997661 ) ) ;
#6197 = CARTESIAN_POINT ( 'NONE',  ( -3.152801135295367985, -21.81250000136559208, 3.152801135295367096 ) ) ;
#6198 = CARTESIAN_POINT ( 'NONE',  ( 3.753672977998667726, 3.033343224707664376, -5.249999998634407028 ) ) ;
#6199 = CARTESIAN_POINT ( 'NONE',  ( 6.000000000000000000, -13.00000000000000178, -1.500000000000000000 ) ) ;
#6200 = EDGE_CURVE ( 'NONE', #1559, #12752, #5124, .T. ) ;
#6201 = ORIENTED_EDGE ( 'NONE', *, *, #8996, .T. ) ;
#6202 = EDGE_LOOP ( 'NONE', ( #15329, #12599, #9206, #13995, #24, #1556, #13140, #1631 ) ) ;
#6203 = EDGE_CURVE ( 'NONE', #7414, #8156, #8213, .T. ) ;
#6204 = DIRECTION ( 'NONE',  ( -0.8660254037844364872, 0.000000000000000000, -0.5000000000000041078 ) ) ;
#6205 = ORIENTED_EDGE ( 'NONE', *, *, #1057, .T. ) ;
#6206 = CARTESIAN_POINT ( 'NONE',  ( 5.000000000000000000, -31.12500000273118772, 0.000000000000000000 ) ) ;
#6207 = DIRECTION ( 'NONE',  ( 0.000000000000000000, -1.000000000000000000, 0.000000000000000000 ) ) ;
#6208 = CARTESIAN_POINT ( 'NONE',  ( 57.73502691896258199, -35.00000000000000000, 2.081668171172168513E-14 ) ) ;
#6209 = DIRECTION ( 'NONE',  ( -1.000000000000000000, 0.000000000000000000, 0.000000000000000000 ) ) ;
#6210 = CARTESIAN_POINT ( 'NONE',  ( -55.00000000000000000, -5.000000000000000000, 19.99999999999999289 ) ) ;
#6211 = CARTESIAN_POINT ( 'NONE',  ( -113.6871902368263250, -110.1917077999037957, 17.50000000000000000 ) ) ;
#6212 = CARTESIAN_POINT ( 'NONE',  ( 5.381735091635035495, -0.5711823568785978633, -0.06250000000000287270 ) ) ;
#6213 = CARTESIAN_POINT ( 'NONE',  ( -5.000000000000091482, -0.7223674278660691117, -2.396799362785969389 ) ) ;
#6214 = CARTESIAN_POINT ( 'NONE',  ( -2.762894178058169725, -3.922440002897376932, -0.1467115563401084066 ) ) ;
#6215 = CARTESIAN_POINT ( 'NONE',  ( 3.152801135295367541, -25.31250000136559564, -3.152801135295367541 ) ) ;
#6216 = CARTESIAN_POINT ( 'NONE',  ( 1.261996585732578113, -4.276409079477644148, -3.812499998634408360 ) ) ;
#6217 = ORIENTED_EDGE ( 'NONE', *, *, #7024, .T. ) ;
#6218 = CARTESIAN_POINT ( 'NONE',  ( -7.500000000000004441, -3.988190556646204588, -0.8526458641284350159 ) ) ;
#6219 = ORIENTED_EDGE ( 'NONE', *, *, #8065, .T. ) ;
#6220 = VERTEX_POINT ( 'NONE', #2430 ) ;
#6221 = EDGE_CURVE ( 'NONE', #11703, #15563, #3656, .T. ) ;
#6222 = CARTESIAN_POINT ( 'NONE',  ( 0.000000000000000000, 40.00000000000000000, 0.000000000000000000 ) ) ;
#6223 = PRODUCT_DEFINITION ( 'UNKNOWN', '', #11789, #12546 ) ;
#6224 = CARTESIAN_POINT ( 'NONE',  ( -3.152801135295367096, -23.06250000136559564, -3.152801135295367541 ) ) ;
#6225 = FACE_OUTER_BOUND ( 'NONE', #4126, .T. ) ;
#6226 = EDGE_LOOP ( 'NONE', ( #6424, #13535, #1856, #4734 ) ) ;
#6227 = DIRECTION ( 'NONE',  ( 0.000000000000000000, 0.000000000000000000, -1.000000000000000000 ) ) ;
#6228 = FACE_OUTER_BOUND ( 'NONE', #11956, .T. ) ;
#6229 = FACE_BOUND ( 'NONE', #11318, .T. ) ;
#6230 = LINE ( 'NONE', #13467, #6797 ) ;
#6231 = CARTESIAN_POINT ( 'NONE',  ( -4.458734124999999437, -24.18750000136559564, -5.460374474430324690E-16 ) ) ;
#6232 = CARTESIAN_POINT ( 'NONE',  ( -99.99999999999998579, -35.00000000000000711, -7.500000000000000000 ) ) ;
#6233 = FACE_OUTER_BOUND ( 'NONE', #11019, .T. ) ;
#6234 = CARTESIAN_POINT ( 'NONE',  ( 5.000000000000000888, -27.06250000273118772, -2.071067811865475505 ) ) ;
#6235 = CARTESIAN_POINT ( 'NONE',  ( -4.795541693661363958, -1.415196051561583790, -6.374999997268815832 ) ) ;
#6236 = CARTESIAN_POINT ( 'NONE',  ( -3.152801135295367985, -28.81250000136559564, 3.152801135295367096 ) ) ;
#6237 = EDGE_CURVE ( 'NONE', #11234, #3134, #35, .T. ) ;
#6238 = CARTESIAN_POINT ( 'NONE',  ( 23.49999999999956657, -8.786575603324269439E-13, -6.000000000000000000 ) ) ;
#6240 = EDGE_CURVE ( 'NONE', #7722, #11193, #11017, .T. ) ;
#6239 = ORIENTED_EDGE ( 'NONE', *, *, #11945, .T. ) ;
#6241 = EDGE_CURVE ( 'NONE', #15294, #12557, #6177, .T. ) ;
#6242 = ORIENTED_EDGE ( 'NONE', *, *, #5041, .F. ) ;
#6243 = DIRECTION ( 'NONE',  ( 0.000000000000000000, 0.000000000000000000, 1.000000000000000000 ) ) ;
#6244 = EDGE_LOOP ( 'NONE', ( #14571, #13955, #6467, #3372 ) ) ;
#6245 = CARTESIAN_POINT ( 'NONE',  ( 0.000000000000000000, 0.000000000000000000, -25.03750572909317285 ) ) ;
#6246 = CARTESIAN_POINT ( 'NONE',  ( 40.27451087355422743, -3.242827243955479943, 27.73563889972393426 ) ) ;
#6247 = CARTESIAN_POINT ( 'NONE',  ( -2.131511515620587272, -3.916244202832140253, -2.687499998634407028 ) ) ;
#6248 = AXIS2_PLACEMENT_3D ( 'NONE', #9547, #10611, #13004 ) ;
#6249 =( LENGTH_UNIT ( ) NAMED_UNIT ( * ) SI_UNIT ( .MILLI., .METRE. ) );
#6250 = CARTESIAN_POINT ( 'NONE',  ( 3.916244202832140253, -2.131511515620588160, -5.687499998634406140 ) ) ;
#6251 = DIRECTION ( 'NONE',  ( 0.000000000000000000, -0.000000000000000000, 1.000000000000000000 ) ) ;
#6252 = CARTESIAN_POINT ( 'NONE',  ( -9.184850993605147944E-16, -24.25000000000000000, 5.000000000000000000 ) ) ;
#6253 = ORIENTED_EDGE ( 'NONE', *, *, #5138, .T. ) ;
#6254 = CARTESIAN_POINT ( 'NONE',  ( -5.725490332117410652, 0.000000000000000000, 9.916840153471811803 ) ) ;
#6255 = EDGE_CURVE ( 'NONE', #6259, #3698, #12291, .T. ) ;
#6256 = VERTEX_POINT ( 'NONE', #4637 ) ;
#6257 = CYLINDRICAL_SURFACE ( 'NONE', #13138, 9.999999999999994671 ) ;
#6258 = DIRECTION ( 'NONE',  ( -0.8660254037844387076, -0.000000000000000000, 0.4999999999999997224 ) ) ;
#6259 = VERTEX_POINT ( 'NONE', #1146 ) ;
#6260 = CARTESIAN_POINT ( 'NONE',  ( 3.033343224707661712, -3.753672977998669502, -1.749999998634408360 ) ) ;
#6261 =( BOUNDED_CURVE ( )  B_SPLINE_CURVE ( 2, ( #5826, #1944, #11877, #13169, #13091, #3397, #3094, #590, #903 ),
 .UNSPECIFIED., .F., .F. ) 
 B_SPLINE_CURVE_WITH_KNOTS ( ( 3, 2, 2, 2, 3 ),
 ( 0.1125000002956211415, 0.1250000000000000000, 0.1375000000000000111, 0.1499999999999999944, 0.1545872658012772960 ),
 .UNSPECIFIED. ) 
 CURVE ( )  GEOMETRIC_REPRESENTATION_ITEM ( )  RATIONAL_B_SPLINE_CURVE ( ( 1.000000000000000000, 0.9238795325112867385, 1.000000000000000000, 0.9238795325112867385, 1.000000000000000000, 0.9238795325112867385, 1.000000000000000000, 0.9720652146169428409, 0.9646335149384808183 ) ) 
 REPRESENTATION_ITEM ( '' )  );
#6262 = DIRECTION ( 'NONE',  ( 0.000000000000000000, 0.000000000000000000, -1.000000000000000000 ) ) ;
#6263 = FACE_OUTER_BOUND ( 'NONE', #13751, .T. ) ;
#6264 = CARTESIAN_POINT ( 'NONE',  ( -1.908195823574487804E-14, -8.660254037844392627, -1.000000000000000888 ) ) ;
#6265 = UNCERTAINTY_MEASURE_WITH_UNIT (LENGTH_MEASURE( 1.000000000000000082E-05 ), #7179, 'distance_accuracy_value', 'NONE');
#6266 = DIRECTION ( 'NONE',  ( -1.000000000000000000, -1.982541115402064863E-16, 0.000000000000000000 ) ) ;
#6267 = CARTESIAN_POINT ( 'NONE',  ( 1.415196051561583790, -4.795541693661363958, -2.124999997268814944 ) ) ;
#6268 = CARTESIAN_POINT ( 'NONE',  ( -44.99999999999999289, -35.00000000000000000, -7.500000000000000000 ) ) ;
#6269 = CARTESIAN_POINT ( 'NONE',  ( -5.000000000000004441, -1.011557177027151181E-15, -6.420263044861759028 ) ) ;
#6270 = CARTESIAN_POINT ( 'NONE',  ( -8.190561711645485556E-16, -23.93750000136559564, 4.458734124999999437 ) ) ;
#6271 = VERTEX_POINT ( 'NONE', #9718 ) ;
#6272 = CARTESIAN_POINT ( 'NONE',  ( 0.000000000000000000, 0.000000000000000000, -4.694516984716113228 ) ) ;
#6273 = CARTESIAN_POINT ( 'NONE',  ( 1.261996585732578113, -4.276409079477644148, -2.562499998634407028 ) ) ;
#6274 = AXIS2_PLACEMENT_3D ( 'NONE', #11327, #12521, #2912 ) ;
#6275 = DIRECTION ( 'NONE',  ( 0.000000000000000000, 0.000000000000000000, 1.000000000000000000 ) ) ;
#6276 = EDGE_LOOP ( 'NONE', ( #15549, #12998, #5429, #5481 ) ) ;
#6277 = CIRCLE ( 'NONE', #15310, 2.500000000000909495 ) ;
#6278 = VERTEX_POINT ( 'NONE', #2201 ) ;
#6279 = CARTESIAN_POINT ( 'NONE',  ( 0.000000000000000000, 0.000000000000000000, 0.000000000000000000 ) ) ;
#6280 = ORIENTED_EDGE ( 'NONE', *, *, #12050, .F. ) ;
#6281 = CARTESIAN_POINT ( 'NONE',  ( 3.061616997868383141E-16, -30.87500000273118772, -5.000000000000000000 ) ) ;
#6282 = CYLINDRICAL_SURFACE ( 'NONE', #11013, 60.00000000000000000 ) ;
#6283 = AXIS2_PLACEMENT_3D ( 'NONE', #2008, #7031, #4437 ) ;
#6284 = CARTESIAN_POINT ( 'NONE',  ( -44.43375672974055846, 0.000000000000000000, 19.99999999999999645 ) ) ;
#6285 = VECTOR ( 'NONE', #15408, 1000.000000000000000 ) ;
#6286 = EDGE_CURVE ( 'NONE', #10095, #13586, #2608, .T. ) ;
#6287 = DIRECTION ( 'NONE',  ( 0.000000000000000000, 0.000000000000000000, 1.000000000000000000 ) ) ;
#6288 = CARTESIAN_POINT ( 'NONE',  ( -7.968863443239230016, -4.547634245050486967, -8.057411785091790790 ) ) ;
#6289 = DIRECTION ( 'NONE',  ( -0.000000000000000000, -1.000000000000000000, -0.000000000000000000 ) ) ;
#6290 = CARTESIAN_POINT ( 'NONE',  ( 2.390265326283148806, 4.391654775818395251, -4.875000000000000888 ) ) ;
#6291 = CARTESIAN_POINT ( 'NONE',  ( 0.000000000000000000, -13.00000000000000178, 0.000000000000000000 ) ) ;
#6292 = CARTESIAN_POINT ( 'NONE',  ( 19.99999999999956657, -8.786575603324269439E-13, 0.000000000000000000 ) ) ;
#6293 = CARTESIAN_POINT ( 'NONE',  ( 4.458734125000000326, -25.37500000136559919, -1.846868145590734978 ) ) ;
#6294 = CARTESIAN_POINT ( 'NONE',  ( -3.753672977998669946, -3.033343224707661712, -3.999999998634410137 ) ) ;
#6295 = ORIENTED_EDGE ( 'NONE', *, *, #12437, .T. ) ;
#6296 = CIRCLE ( 'NONE', #12460, 27.99999999999998934 ) ;
#6297 = DIRECTION ( 'NONE',  ( -0.8660254037844387076, -0.000000000000000000, 0.4999999999999997224 ) ) ;
#6298 = ORIENTED_EDGE ( 'NONE', *, *, #6525, .T. ) ;
#6299 = ORIENTED_EDGE ( 'NONE', *, *, #13497, .F. ) ;
#6300 = CARTESIAN_POINT ( 'NONE',  ( -4.000000000000000000, -0.8382240730041925492, -3.220610619767135141 ) ) ;
#6301 = CARTESIAN_POINT ( 'NONE',  ( 4.458734125000000326, -26.37500000136559564, -1.846868145590734978 ) ) ;
#6302 = DIRECTION ( 'NONE',  ( 0.000000000000000000, -1.387778780781445676E-15, -1.000000000000000000 ) ) ;
#6303 = ORIENTED_EDGE ( 'NONE', *, *, #473, .F. ) ;
#6304 = CARTESIAN_POINT ( 'NONE',  ( 2.602085213965210642E-15, 8.660254037844392627, -7.422398894150035176 ) ) ;
#6305 = DIRECTION ( 'NONE',  ( 0.000000000000000000, 0.000000000000000000, -1.000000000000000000 ) ) ;
#6306 = EDGE_CURVE ( 'NONE', #6165, #9005, #3490, .T. ) ;
#6307 = CARTESIAN_POINT ( 'NONE',  ( 2.131511515620586383, 3.916244202832140253, -3.187499998634407916 ) ) ;
#6308 = CARTESIAN_POINT ( 'NONE',  ( -31.74999999999995737, 0.000000000000000000, 0.000000000000000000 ) ) ;
#6309 = EDGE_CURVE ( 'NONE', #2513, #2071, #4950, .T. ) ;
#6310 = CARTESIAN_POINT ( 'NONE',  ( 3.061616997868383141E-16, -31.75000000000000000, -5.000000000000000000 ) ) ;
#6311 = CARTESIAN_POINT ( 'NONE',  ( -2.886751345948099789, -4.999999999999997335, -35.00000000000000000 ) ) ;
#6312 = DIRECTION ( 'NONE',  ( -0.000000000000000000, 1.000000000000000000, -0.000000000000000000 ) ) ;
#6313 = CARTESIAN_POINT ( 'NONE',  ( 3.061616997868383141E-16, -28.87500000273118772, -5.000000000000000000 ) ) ;
#6314 = CARTESIAN_POINT ( 'NONE',  ( 4.606548227981507537, 6.456511556909250160, -7.591235721156634142 ) ) ;
#6315 = COLOUR_RGB ( '', 0.66274510, 0.83137255, 0.94901961) ;
#6316 = CARTESIAN_POINT ( 'NONE',  ( 2.500000000000000000, 2.357898499370433054, -1.951563910473907981E-15 ) ) ;
#6317 = ORIENTED_EDGE ( 'NONE', *, *, #13380, .T. ) ;
#6318 = ORIENTED_EDGE ( 'NONE', *, *, #1179, .F. ) ;
#6319 = VERTEX_POINT ( 'NONE', #8599 ) ;
#6320 = CARTESIAN_POINT ( 'NONE',  ( 19.99999999999956657, -8.786575603324269439E-13, 0.000000000000000000 ) ) ;
#6321 = VERTEX_POINT ( 'NONE', #14810 ) ;
#6322 = DIRECTION ( 'NONE',  ( 0.000000000000000000, 1.000000000000000000, 0.000000000000000000 ) ) ;
#6323 = COLOUR_RGB ( '', 0.08235294, 0.09019608, 0.10196078) ;
#6324 = EDGE_CURVE ( 'NONE', #869, #14231, #6087, .T. ) ;
#6325 = ADVANCED_FACE ( 'NONE', ( #5934 ), #9252, .F. ) ;
#6326 = AXIS2_PLACEMENT_3D ( 'NONE', #7102, #8555, #1098 ) ;
#6327 = CARTESIAN_POINT ( 'NONE',  ( 35.00000000000000000, 37.00000000000000000, -8.572527594031472993E-15 ) ) ;
#6328 = CARTESIAN_POINT ( 'NONE',  ( -3.033343224707664376, 3.753672977998667726, -1.999999998634408360 ) ) ;
#6329 = CARTESIAN_POINT ( 'NONE',  ( -4.276409079477644148, -1.261996585732578335, -5.062499998634406140 ) ) ;
#6330 = CYLINDRICAL_SURFACE ( 'NONE', #5107, 2.649999999999985700 ) ;
#6331 = CARTESIAN_POINT ( 'NONE',  ( 4.535975386569504053, 1.338596318647080397, -8.156249999317205734 ) ) ;
#6332 = ORIENTED_EDGE ( 'NONE', *, *, #15712, .T. ) ;
#6333 = CARTESIAN_POINT ( 'NONE',  ( -7.500000000000003553, -1.443375672974066770, -7.063244554130003294 ) ) ;
#6334 = VECTOR ( 'NONE', #11893, 1000.000000000000227 ) ;
#6335 = ORIENTED_EDGE ( 'NONE', *, *, #2731, .F. ) ;
#6336 = CARTESIAN_POINT ( 'NONE',  ( 4.000000000000000000, 2.512223110932545023, -3.469391141908803711 ) ) ;
#6337 = DIRECTION ( 'NONE',  ( 0.000000000000000000, 0.000000000000000000, 1.000000000000000000 ) ) ;
#6338 = COLOUR_RGB ( '', 0.40784314, 0.44705882, 0.49803922) ;
#6339 = ORIENTED_EDGE ( 'NONE', *, *, #4976, .T. ) ;
#6340 = CARTESIAN_POINT ( 'NONE',  ( -1.261996585732579224, 4.276409079477648589, -8.312499998634407916 ) ) ;
#6341 = EDGE_CURVE ( 'NONE', #7945, #14772, #10783, .T. ) ;
#6342 = AXIS2_PLACEMENT_3D ( 'NONE', #9535, #14385, #10977 ) ;
#6343 = DIRECTION ( 'NONE',  ( -1.000000000000000000, -0.000000000000000000, -0.000000000000000000 ) ) ;
#6344 = DIRECTION ( 'NONE',  ( -0.000000000000000000, 1.000000000000000000, -0.000000000000000000 ) ) ;
#6345 = VECTOR ( 'NONE', #14723, 1000.000000000000000 ) ;
#6346 = CARTESIAN_POINT ( 'NONE',  ( 5.000000000000000888, -27.06250000273118772, -2.071067811865475505 ) ) ;
#6347 = AXIS2_PLACEMENT_3D ( 'NONE', #13310, #1046, #15844 ) ;
#6348 = CARTESIAN_POINT ( 'NONE',  ( 2.390265326283148806, 4.391654775818395251, -3.749999997268816720 ) ) ;
#6349 = CARTESIAN_POINT ( 'NONE',  ( -5.000000000000000888, -23.56250000000000000, -2.071067811865475949 ) ) ;
#6350 = CARTESIAN_POINT ( 'NONE',  ( 19.99999999999956657, -8.786575603324269439E-13, 1.500000000000000000 ) ) ;
#6351 = CARTESIAN_POINT ( 'NONE',  ( -1.846868145590734756, -22.37500000136559564, -4.458734124999999437 ) ) ;
#6352 = ORIENTED_EDGE ( 'NONE', *, *, #3986, .T. ) ;
#6353 = CARTESIAN_POINT ( 'NONE',  ( 33.48631561299829684, -3.000000000000000000, 14.00000000000000888 ) ) ;
#6354 = CARTESIAN_POINT ( 'NONE',  ( 4.276409079477644148, 1.261996585732577891, -6.312499998634407028 ) ) ;
#6355 = LINE ( 'NONE', #2537, #15909 ) ;
#6356 = ORIENTED_EDGE ( 'NONE', *, *, #9392, .T. ) ;
#6357 = VERTEX_POINT ( 'NONE', #13343 ) ;
#6358 =( BOUNDED_CURVE ( )  B_SPLINE_CURVE ( 2, ( #4112, #2732, #5330, #8816, #258, #15195, #5173, #13718, #13795, #7690, #12587, #6543, #1532, #11540, #5088, #2572, #7602, #11307, #11460, #407, #10101, #9060, #11382, #15034, #8976, #3948, #13962, #15275, #6470, #11224, #13888, #333, #5247, #1686, #6627, #10183, #2819, #490, #10269, #10348, #10022, #5414, #9135, #7523, #12426, #1359, #6307, #169, #14959, #3874, #3140, #3216, #12906, #1840, #13147, #12824, #1918, #10419, #568, #4272, #3065, #2080, #8164, #726, #10506, #5650, #10593, #11617, #15517, #4433, #2003, #10734, #5489, #8253, #7026, #878, #10657, #15354, #9213, #8009, #11927, #5721, #14137, #6715, #14047, #9368, #6784, #15440, #11692, #14372, #14292, #647, #5570, #15590, #4362, #9297, #6952, #1768, #2972, #14220, #8087, #11772, #13065, #12982, #11854, #6866, #802, #4508, #5797, #9444, #3301, #7926, #15672, #4587, #12383, #9813, #13677, #7561, #14911, #1081, #15147, #14371, #12459, #7396, #3744, #10942, #6019, #2524, #3666 ),
 .UNSPECIFIED., .F., .F. ) 
 B_SPLINE_CURVE_WITH_KNOTS ( ( 3, 2, 2, 2, 2, 2, 2, 2, 2, 2, 2, 2, 2, 2, 2, 2, 2, 2, 2, 2, 2, 2, 2, 2, 2, 2, 2, 2, 2, 2, 2, 2, 2, 2, 2, 2, 2, 2, 2, 2, 2, 2, 2, 2, 2, 2, 2, 2, 2, 2, 2, 2, 2, 2, 2, 2, 2, 2, 2, 2, 2, 2, 2, 2, 3 ),
 ( 0.2066346841896726794, 0.2124999999999999944, 0.2250000000000000056, 0.2374999999999999889, 0.2500000000000000000, 0.2625000000000000111, 0.2750000000000000222, 0.2874999999999999778, 0.2999999999999999889, 0.3125000000000000000, 0.3250000000000000111, 0.3375000000000000222, 0.3499999999999999778, 0.3624999999999999889, 0.3750000000000000000, 0.3875000000000000666, 0.4000000000000000222, 0.4124999999999999778, 0.4249999999999999889, 0.4375000000000000000, 0.4500000000000000666, 0.4625000000000000222, 0.4749999999999999778, 0.4874999999999999889, 0.5000000000000000000, 0.5124999999999999556, 0.5250000000000000222, 0.5374999999999998668, 0.5500000000000000444, 0.5625000000000000000, 0.5749999999999999556, 0.5875000000000000222, 0.5999999999999999778, 0.6125000000000000444, 0.6250000000000000000, 0.6374999999999999556, 0.6500000000000000222, 0.6624999999999998668, 0.6750000000000000444, 0.6875000000000000000, 0.6999999999999999556, 0.7125000000000000222, 0.7249999999999999778, 0.7375000000000000444, 0.7500000000000000000, 0.7624999999999999556, 0.7750000000000000222, 0.7874999999999999778, 0.8000000000000000444, 0.8125000000000000000, 0.8249999999999999556, 0.8375000000000000222, 0.8499999999999999778, 0.8625000000000000444, 0.8749999999999998890, 0.8874999999999999556, 0.9000000000000000222, 0.9124999999999999778, 0.9250000000000000444, 0.9375000000000000000, 0.9499999999999999556, 0.9625000000000000222, 0.9749999999999998668, 0.9875000000000001554, 1.000000000000000000 ),
 .UNSPECIFIED. ) 
 CURVE ( )  GEOMETRIC_REPRESENTATION_ITEM ( )  RATIONAL_B_SPLINE_CURVE ( ( 0.9620839512587866516, 0.9642823534839154442, 1.000000000000000000, 0.9238795325112867385, 1.000000000000000000, 0.9238795325112867385, 1.000000000000000000, 0.9238795325112867385, 1.000000000000000000, 0.9238795325112867385, 1.000000000000000000, 0.9238795325112867385, 1.000000000000000000, 0.9238795325112867385, 1.000000000000000000, 0.9238795325112867385, 1.000000000000000000, 0.9238795325112867385, 1.000000000000000000, 0.9238795325112867385, 1.000000000000000000, 0.9238795325112867385, 1.000000000000000000, 0.9238795325112867385, 1.000000000000000000, 0.9238795325112867385, 1.000000000000000000, 0.9238795325112867385, 1.000000000000000000, 0.9238795325112867385, 1.000000000000000000, 0.9238795325112867385, 1.000000000000000000, 0.9238795325112867385, 1.000000000000000000, 0.9238795325112867385, 1.000000000000000000, 0.9238795325112867385, 1.000000000000000000, 0.9238795325112867385, 1.000000000000000000, 0.9238795325112867385, 1.000000000000000000, 0.9238795325112867385, 1.000000000000000000, 0.9238795325112867385, 1.000000000000000000, 0.9238795325112867385, 1.000000000000000000, 0.9238795325112867385, 1.000000000000000000, 0.9238795325112867385, 1.000000000000000000, 0.9238795325112867385, 1.000000000000000000, 0.9238795325112867385, 1.000000000000000000, 0.9238795325112867385, 1.000000000000000000, 0.9238795325112867385, 1.000000000000000000, 0.9238795325112867385, 1.000000000000000000, 0.9238795325112867385, 1.000000000000000000, 0.9238795325112867385, 1.000000000000000000, 0.9238795325112867385, 1.000000000000000000, 0.9238795325112867385, 1.000000000000000000, 0.9238795325112867385, 1.000000000000000000, 0.9238795325112867385, 1.000000000000000000, 0.9238795325112867385, 1.000000000000000000, 0.9238795325112867385, 1.000000000000000000, 0.9238795325112867385, 1.000000000000000000, 0.9238795325112867385, 1.000000000000000000, 0.9238795325112867385, 1.000000000000000000, 0.9238795325112867385, 1.000000000000000000, 0.9238795325112867385, 1.000000000000000000, 0.9238795325112867385, 1.000000000000000000, 0.9238795325112867385, 1.000000000000000000, 0.9238795325112867385, 1.000000000000000000, 0.9238795325112867385, 1.000000000000000000, 0.9238795325112867385, 1.000000000000000000, 0.9238795325112867385, 1.000000000000000000, 0.9238795325112867385, 1.000000000000000000, 0.9238795325112867385, 1.000000000000000000, 0.9238795325112867385, 1.000000000000000000, 0.9238795325112867385, 1.000000000000000000, 0.9238795325112867385, 1.000000000000000000, 0.9238795325112867385, 1.000000000000000000, 0.9238795325112867385, 1.000000000000000000, 0.9238795325112867385, 1.000000000000000000, 0.9238795325112867385, 1.000000000000000000, 0.9238795325112867385, 1.000000000000000000, 0.9238795325112867385, 1.000000000000000000, 0.9238795325112867385, 1.000000000000000000, 0.9238795325112867385, 1.000000000000000000, 0.9238795325112867385, 1.000000000000000000 ) ) 
 REPRESENTATION_ITEM ( '' )  );
#6360 = VECTOR ( 'NONE', #4237, 1000.000000000000000 ) ;
#6359 = DIRECTION ( 'NONE',  ( 0.000000000000000000, 0.000000000000000000, 1.000000000000000000 ) ) ;
#6361 = ORIENTED_EDGE ( 'NONE', *, *, #5361, .T. ) ;
#6362 = CARTESIAN_POINT ( 'NONE',  ( 5.000000000000004441, 3.034671531081452754E-15, -0.04526304759294640795 ) ) ;
#6363 = FACE_OUTER_BOUND ( 'NONE', #8684, .T. ) ;
#6364 = CIRCLE ( 'NONE', #5589, 0.5155456020628804703 ) ;
#6365 = CARTESIAN_POINT ( 'NONE',  ( -43.85680617778868395, -3.000000000000000000, -22.00000000000000355 ) ) ;
#6366 = EDGE_CURVE ( 'NONE', #11846, #13350, #2274, .T. ) ;
#6367 = CARTESIAN_POINT ( 'NONE',  ( 19.99999999999956657, -8.786575603324269439E-13, 0.000000000000000000 ) ) ;
#6369 = CARTESIAN_POINT ( 'NONE',  ( -0.3875187462258835036, -8.436519985396071064, -7.781689322727316060 ) ) ;
#6368 =( GEOMETRIC_REPRESENTATION_CONTEXT ( 3 ) GLOBAL_UNCERTAINTY_ASSIGNED_CONTEXT ( ( #2883 ) ) GLOBAL_UNIT_ASSIGNED_CONTEXT ( ( #13339, #14808, #9803 ) ) REPRESENTATION_CONTEXT ( 'NONE', 'WORKASPACE' ) );
#6370 = DIRECTION ( 'NONE',  ( -0.000000000000000000, 0.8660254037844390407, 0.4999999999999993339 ) ) ;
#6371 = CARTESIAN_POINT ( 'NONE',  ( -4.209348295687703967, -3.401574460001763001, -3.437500000000003553 ) ) ;
#6372 = CARTESIAN_POINT ( 'NONE',  ( 5.000000000000000000, -30.00000000000000000, 0.000000000000000000 ) ) ;
#6373 = DIRECTION ( 'NONE',  ( 0.000000000000000000, 0.000000000000000000, 1.000000000000000000 ) ) ;
#6374 = CARTESIAN_POINT ( 'NONE',  ( 1.846868145590736310, -26.62500000136559564, 4.458734124999999437 ) ) ;
#6375 = CARTESIAN_POINT ( 'NONE',  ( 0.5093500532425063732, 4.799145180956616130, -2.374999998634407028 ) ) ;
#6376 = ORIENTED_EDGE ( 'NONE', *, *, #12142, .T. ) ;
#6377 = VECTOR ( 'NONE', #7724, 1000.000000000000000 ) ;
#6378 = LINE ( 'NONE', #5165, #11998 ) ;
#6379 = ORIENTED_EDGE ( 'NONE', *, *, #11874, .F. ) ;
#6380 = EDGE_LOOP ( 'NONE', ( #8663, #11359, #11699, #561 ) ) ;
#6381 = CARTESIAN_POINT ( 'NONE',  ( -1.846868145590734756, -26.12500000136559564, -4.458734125000000326 ) ) ;
#6382 = ADVANCED_FACE ( 'NONE', ( #11971 ), #924, .T. ) ;
#6383 = CYLINDRICAL_SURFACE ( 'NONE', #2994, 31.99999999999999289 ) ;
#6384 = AXIS2_PLACEMENT_3D ( 'NONE', #2549, #5305, #13942 ) ;
#6385 = ORIENTED_EDGE ( 'NONE', *, *, #3426, .T. ) ;
#6386 = CARTESIAN_POINT ( 'NONE',  ( -4.000000000000000000, -0.7890432684750890990, -0.04868663549882315533 ) ) ;
#6387 = PRODUCT_DEFINITION_FORMATION_WITH_SPECIFIED_SOURCE ( 'ANY', '', #4208, .NOT_KNOWN. ) ;
#6388 = DIRECTION ( 'NONE',  ( 1.000000000000000000, 0.000000000000000000, 0.000000000000000000 ) ) ;
#6389 = CYLINDRICAL_SURFACE ( 'NONE', #3946, 2.649999999999992806 ) ;
#6390 = ADVANCED_BREP_SHAPE_REPRESENTATION ( '', ( #3780, #3223 ), #8900 ) ;
#6391 = CARTESIAN_POINT ( 'NONE',  ( -2.071067811865475061, -31.68750000000000000, -5.000000000000000888 ) ) ;
#6392 = DIRECTION ( 'NONE',  ( 1.000000000000000000, -6.938893903907232322E-16, 0.000000000000000000 ) ) ;
#6393 = DIRECTION ( 'NONE',  ( -0.000000000000000000, -0.000000000000000000, 1.000000000000000000 ) ) ;
#6394 = CARTESIAN_POINT ( 'NONE',  ( 2.071067811865476394, -30.31250000273118772, 5.000000000000000000 ) ) ;
#6395 = FACE_OUTER_BOUND ( 'NONE', #14036, .T. ) ;
#6396 = CARTESIAN_POINT ( 'NONE',  ( 2.071067811865475505, -23.93750000273119127, -5.000000000000000888 ) ) ;
#6397 = FILL_AREA_STYLE ('',( #12274 ) ) ;
#6398 = EDGE_LOOP ( 'NONE', ( #13187, #3055, #2204, #4450 ) ) ;
#6399 = VERTEX_POINT ( 'NONE', #1070 ) ;
#6400 = AXIS2_PLACEMENT_3D ( 'NONE', #6828, #11736, #6756 ) ;
#6401 = AXIS2_PLACEMENT_3D ( 'NONE', #3032, #13771, #10240 ) ;
#6403 = ORIENTED_EDGE ( 'NONE', *, *, #8676, .T. ) ;
#6402 = ADVANCED_FACE ( 'NONE', ( #15955 ), #6412, .T. ) ;
#6404 = PLANE ( 'NONE',  #5578 ) ;
#6405 = EDGE_CURVE ( 'NONE', #8017, #2243, #15218, .T. ) ;
#6406 = ORIENTED_EDGE ( 'NONE', *, *, #8377, .T. ) ;
#6407 = FACE_OUTER_BOUND ( 'NONE', #15268, .T. ) ;
#6408 = AXIS2_PLACEMENT_3D ( 'NONE', #1385, #13740, #1305 ) ;
#6409 =( REPRESENTATION_RELATIONSHIP ('NONE','NONE', #4176, #1906 ) REPRESENTATION_RELATIONSHIP_WITH_TRANSFORMATION ( #7557 )SHAPE_REPRESENTATION_RELATIONSHIP( ) );
#6410 = CARTESIAN_POINT ( 'NONE',  ( 7.894787914004607998, 0.7661396099416303285, -7.591390474663427312 ) ) ;
#6411 = CARTESIAN_POINT ( 'NONE',  ( -55.00000000000000000, 0.000000000000000000, -18.00000000000001066 ) ) ;
#6412 = CONICAL_SURFACE ( 'NONE', #7202, 7.500000000000001776, 0.8594454914424796144 ) ;
#6413 = CARTESIAN_POINT ( 'NONE',  ( -3.753672977998669946, -3.033343224707661712, -4.999999998634407028 ) ) ;
#6414 = DIRECTION ( 'NONE',  ( 0.000000000000000000, 1.000000000000000000, 0.000000000000000000 ) ) ;
#6415 = CIRCLE ( 'NONE', #2792, 31.99999999999999289 ) ;
#6416 = FACE_OUTER_BOUND ( 'NONE', #2147, .T. ) ;
#6417 = ORIENTED_EDGE ( 'NONE', *, *, #4639, .F. ) ;
#6418 = DIRECTION ( 'NONE',  ( 0.000000000000000000, 0.000000000000000000, 1.000000000000000000 ) ) ;
#6419 = AXIS2_PLACEMENT_3D ( 'NONE', #13341, #5848, #13256 ) ;
#6420 = ORIENTED_EDGE ( 'NONE', *, *, #3255, .T. ) ;
#6421 = DIRECTION ( 'NONE',  ( -0.000000000000000000, 0.8660254037844390407, 0.4999999999999993339 ) ) ;
#6422 = CARTESIAN_POINT ( 'NONE',  ( 0.000000000000000000, -13.00000000000000178, 1.500000000000000000 ) ) ;
#6423 = ADVANCED_FACE ( 'NONE', ( #3895 ), #13916, .T. ) ;
#6424 = ORIENTED_EDGE ( 'NONE', *, *, #9478, .F. ) ;
#6425 = CONTEXT_DEPENDENT_SHAPE_REPRESENTATION ( #7236, #15419 ) ;
#6426 = CARTESIAN_POINT ( 'NONE',  ( 1.261996585732578113, -4.276409079477644148, -7.812499998634407916 ) ) ;
#6427 = CARTESIAN_POINT ( 'NONE',  ( -4.391654775818395251, 2.390265326283148806, -4.499999997268817609 ) ) ;
#6428 = VECTOR ( 'NONE', #4534, 1000.000000000000000 ) ;
#6429 = AXIS2_PLACEMENT_3D ( 'NONE', #1358, #8974, #10020 ) ;
#6430 = CARTESIAN_POINT ( 'NONE',  ( -5.000000000000000888, -28.56250000273119127, 2.071067811865474617 ) ) ;
#6431 = LINE ( 'NONE', #1320, #721 ) ;
#6432 = PRODUCT_DEFINITION_CONTEXT ( 'detailed design', #3609, 'design' ) ;
#6433 = CARTESIAN_POINT ( 'NONE',  ( -0.6666666666666651864, 4.233901974057260098, -3.300726591567081147 ) ) ;
#6434 = VECTOR ( 'NONE', #12164, 1000.000000000000000 ) ;
#6435 = CARTESIAN_POINT ( 'NONE',  ( 0.5711823568785989735, 5.381735091635026613, -4.687499997268819385 ) ) ;
#6436 = CARTESIAN_POINT ( 'NONE',  ( 0.2500000000000002220, 5.204748896376250699E-16, -4.250000000000000000 ) ) ;
#6437 = CARTESIAN_POINT ( 'NONE',  ( -39.99999999999999289, -11.00000000000000178, 8.300651832549021947E-13 ) ) ;
#6438 = VERTEX_POINT ( 'NONE', #7719 ) ;
#6439 = DIRECTION ( 'NONE',  ( 1.000000000000000000, 1.734723475976806848E-16, 0.000000000000000000 ) ) ;
#6440 = CARTESIAN_POINT ( 'NONE',  ( -5.725490332117410652, -3.000000000000000000, 9.916840153471811803 ) ) ;
#6441 = DIRECTION ( 'NONE',  ( 0.000000000000000000, -0.000000000000000000, -1.000000000000000000 ) ) ;
#6442 = EDGE_CURVE ( 'NONE', #2328, #13050, #2786, .T. ) ;
#6443 = ORIENTED_EDGE ( 'NONE', *, *, #12894, .T. ) ;
#6444 = EDGE_LOOP ( 'NONE', ( #2702, #4375 ) ) ;
#6445 = EDGE_CURVE ( 'NONE', #742, #14284, #11807, .T. ) ;
#6446 = EDGE_CURVE ( 'NONE', #2074, #2190, #110, .T. ) ;
#6447 = ORIENTED_EDGE ( 'NONE', *, *, #586, .F. ) ;
#6448 = CARTESIAN_POINT ( 'NONE',  ( -3.333333333333332149, -2.694301256218264218, -3.300726591567082036 ) ) ;
#6449 = DIRECTION ( 'NONE',  ( 0.000000000000000000, 0.4999999999999993339, -0.8660254037844390407 ) ) ;
#6450 = CARTESIAN_POINT ( 'NONE',  ( -5.000000000000000888, -27.56250000273118772, 2.071067811865474617 ) ) ;
#6451 = LINE ( 'NONE', #11363, #6639 ) ;
#6452 = CARTESIAN_POINT ( 'NONE',  ( -2.387978478801059179, -7.281554020289573437, -7.069802615102041443 ) ) ;
#6453 = DIRECTION ( 'NONE',  ( 0.000000000000000000, -0.4999999999999992784, 0.8660254037844389297 ) ) ;
#6454 = CARTESIAN_POINT ( 'NONE',  ( -4.795541693661363958, -1.415196051561583790, -5.500000000000001776 ) ) ;
#6455 = CARTESIAN_POINT ( 'NONE',  ( 5.000000000000095923, 0.7223674278660565662, -3.021799365517156666 ) ) ;
#6456 = LINE ( 'NONE', #2555, #11811 ) ;
#6457 = CARTESIAN_POINT ( 'NONE',  ( -4.458734124999999437, -21.93750000136559208, -5.460374474430324690E-16 ) ) ;
#6458 =( BOUNDED_CURVE ( )  B_SPLINE_CURVE ( 2, ( #8768, #3494, #8452, #8531, #6181, #13348, #7239, #7309, #10303, #13993, #5274 ),
 .UNSPECIFIED., .F., .F. ) 
 B_SPLINE_CURVE_WITH_KNOTS ( ( 3, 2, 2, 2, 2, 3 ),
 ( 0.3045872658012772627, 0.3125000000000000000, 0.3250000000000000111, 0.3375000000000000222, 0.3499999999999999778, 0.3545872658012772516 ),
 .UNSPECIFIED. ) 
 CURVE ( )  GEOMETRIC_REPRESENTATION_ITEM ( )  RATIONAL_B_SPLINE_CURVE ( ( 0.9646335149384808183, 0.9518143178943437865, 1.000000000000000000, 0.9238795325112867385, 1.000000000000000000, 0.9238795325112867385, 1.000000000000000000, 0.9238795325112867385, 1.000000000000000000, 0.9720652146169430630, 0.9646335149384808183 ) ) 
 REPRESENTATION_ITEM ( '' )  );
#6459 = CARTESIAN_POINT ( 'NONE',  ( 4.799145180956616130, -0.5093500532425063732, -6.624999998634407916 ) ) ;
#6460 = EDGE_LOOP ( 'NONE', ( #8530, #13959, #2992, #9314, #15800 ) ) ;
#6461 = CARTESIAN_POINT ( 'NONE',  ( -7.894787914004613327, -1.222495057920810896E-13, -7.591390474663425536 ) ) ;
#6462 = VERTEX_POINT ( 'NONE', #9960 ) ;
#6463 = ORIENTED_EDGE ( 'NONE', *, *, #3631, .T. ) ;
#6464 = EDGE_CURVE ( 'NONE', #7075, #4563, #157, .T. ) ;
#6465 = CARTESIAN_POINT ( 'NONE',  ( 4.458734125000000326, -30.62500000136559208, -1.846868145590734978 ) ) ;
#6466 = DIRECTION ( 'NONE',  ( -0.000000000000000000, 1.000000000000000000, -0.000000000000000000 ) ) ;
#6467 = ORIENTED_EDGE ( 'NONE', *, *, #12564, .T. ) ;
#6468 = CARTESIAN_POINT ( 'NONE',  ( 3.061616997868383141E-16, -28.75000000000000000, -5.000000000000000000 ) ) ;
#6469 = CARTESIAN_POINT ( 'NONE',  ( 0.000000000000000000, 0.000000000000000000, -4.974599999999998801 ) ) ;
#6470 = CARTESIAN_POINT ( 'NONE',  ( -1.261996585732579224, 4.276409079477648589, -2.062499998634406584 ) ) ;
#6471 = CARTESIAN_POINT ( 'NONE',  ( 2.143131898507869826E-15, 50.00000000000000000, -67.50000000000000000 ) ) ;
#6472 = CARTESIAN_POINT ( 'NONE',  ( -5.000000000000000000, -31.50000000000000000, -6.123233995736766282E-16 ) ) ;
#6473 = CARTESIAN_POINT ( 'NONE',  ( -6.250000000000000888, -5.051814855409232585, -7.198902722707430257 ) ) ;
#6474 = CARTESIAN_POINT ( 'NONE',  ( -1.154700538379252350, 1.999999999999994893, 34.00000000000000000 ) ) ;
#6475 = CARTESIAN_POINT ( 'NONE',  ( -5.000000000000000000, -23.62500000273118772, -6.123233995736766282E-16 ) ) ;
#6476 = CARTESIAN_POINT ( 'NONE',  ( -41.99999999999978684, -9.000000000000001776, 1.499999999999999112 ) ) ;
#6477 = CARTESIAN_POINT ( 'NONE',  ( 1.846868145590735200, -31.25000000136559564, -4.458734124999999437 ) ) ;
#6478 = CARTESIAN_POINT ( 'NONE',  ( 4.000000000000000000, -2.309401076758516691, -0.4999999999999995559 ) ) ;
#6479 = ORIENTED_EDGE ( 'NONE', *, *, #3613, .T. ) ;
#6480 = ORIENTED_EDGE ( 'NONE', *, *, #2569, .F. ) ;
#6481 =( LENGTH_UNIT ( ) NAMED_UNIT ( * ) SI_UNIT ( .MILLI., .METRE. ) );
#6482 = ORIENTED_EDGE ( 'NONE', *, *, #5804, .T. ) ;
#6483 = CARTESIAN_POINT ( 'NONE',  ( 4.000000000000000000, -2.309401076758514915, -3.433295621305383349 ) ) ;
#6484 = EDGE_LOOP ( 'NONE', ( #2762, #10627, #3756 ) ) ;
#6485 = CARTESIAN_POINT ( 'NONE',  ( 0.000000000000000000, -20.00000000000000000, 5.000000000000000000 ) ) ;
#6486 = B_SPLINE_CURVE_WITH_KNOTS ( 'NONE', 3,
 ( #3159, #5590, #3394, #978, #900, #15610, #5743, #10527, #12924, #15461, #14397, #2176, #15775, #4382, #6805, #9316 ),
 .UNSPECIFIED., .F., .F.,
 ( 4, 2, 2, 2, 2, 2, 2, 4 ),
 ( 0.000000000000000000, 0.0003988081628697240084, 0.0007976163257394480169, 0.001196424488609171971, 0.001595232651478896034, 0.001994040814348619229, 0.002392848977218342207, 0.003190465302957785562 ),
 .UNSPECIFIED. ) ;
#6487 = CARTESIAN_POINT ( 'NONE',  ( -1.415196051561583790, 4.795541693661363958, -1.624999997268814722 ) ) ;
#6488 = DIRECTION ( 'NONE',  ( -0.000000000000000000, 1.000000000000000000, -0.000000000000000000 ) ) ;
#6489 = CARTESIAN_POINT ( 'NONE',  ( 35.00000000000000000, 37.00000000000000000, 5.999999999999991118 ) ) ;
#6490 = EDGE_CURVE ( 'NONE', #10322, #7200, #10052, .T. ) ;
#6491 = EDGE_CURVE ( 'NONE', #2220, #11871, #12583, .T. ) ;
#6492 = APPLICATION_PROTOCOL_DEFINITION ( 'draft international standard', 'automotive_design', 1998, #14352 ) ;
#6493 = CARTESIAN_POINT ( 'NONE',  ( -1.261996585732579224, 4.276409079477648589, -6.312499998634407028 ) ) ;
#6494 = DIRECTION ( 'NONE',  ( 1.000000000000000000, 0.000000000000000000, -0.000000000000000000 ) ) ;
#6495 = ORIENTED_EDGE ( 'NONE', *, *, #11960, .T. ) ;
#6496 = DIRECTION ( 'NONE',  ( 0.000000000000000000, -1.000000000000000000, 0.000000000000000000 ) ) ;
#6497 = ORIENTED_EDGE ( 'NONE', *, *, #15255, .T. ) ;
#6498 = CARTESIAN_POINT ( 'NONE',  ( -2.390265326283148806, -4.391654775818394363, -7.375000000000002665 ) ) ;
#6499 = CARTESIAN_POINT ( 'NONE',  ( 7.347880794884118356E-15, 0.000000000000000000, 60.00000000000000000 ) ) ;
#6500 = EDGE_LOOP ( 'NONE', ( #11006, #3678 ) ) ;
#6501 = ITEM_DEFINED_TRANSFORMATION ( 'NONE', 'NONE', #2420,  #3223 ) ;
#6502 = CARTESIAN_POINT ( 'NONE',  ( 2.131511515620586383, 3.916244202832140253, -7.437499998634407916 ) ) ;
#6503 = PLANE ( 'NONE',  #13028 ) ;
#6504 = CARTESIAN_POINT ( 'NONE',  ( 4.762271716570388058, 0.4578986391487566143, -0.1664591361020693883 ) ) ;
#6505 = EDGE_CURVE ( 'NONE', #5600, #12918, #11337, .T. ) ;
#6506 = CARTESIAN_POINT ( 'NONE',  ( 19.99999999999956657, -8.786575603324269439E-13, -6.000000000000000000 ) ) ;
#6507 = ADVANCED_FACE ( 'NONE', ( #10127 ), #15058, .F. ) ;
#6508 = CARTESIAN_POINT ( 'NONE',  ( 4.795541693661363958, 1.415196051561583790, -2.874999997268815832 ) ) ;
#6509 = CARTESIAN_POINT ( 'NONE',  ( -2.071067811865478170, -23.31249999999999645, 5.000000000000000000 ) ) ;
#6510 = DIRECTION ( 'NONE',  ( 0.000000000000000000, 0.000000000000000000, 1.000000000000000000 ) ) ;
#6511 = CARTESIAN_POINT ( 'NONE',  ( -3.152801135295367985, -22.06250000136559564, 3.152801135295367096 ) ) ;
#6512 = ORIENTED_EDGE ( 'NONE', *, *, #5416, .F. ) ;
#6513 = CARTESIAN_POINT ( 'NONE',  ( -55.00000000000000000, -9.999999999999996447, 7.500000000000001776 ) ) ;
#6514 = CARTESIAN_POINT ( 'NONE',  ( 7.499999999999999112, -1.443375672974070101, -7.063244554130002406 ) ) ;
#6515 = FACE_OUTER_BOUND ( 'NONE', #3514, .T. ) ;
#6516 = EDGE_LOOP ( 'NONE', ( #5297, #4242 ) ) ;
#6517 = ORIENTED_EDGE ( 'NONE', *, *, #7135, .F. ) ;
#6518 = EDGE_LOOP ( 'NONE', ( #3192, #11357, #8624, #6881 ) ) ;
#6519 = CARTESIAN_POINT ( 'NONE',  ( 6.123233995736766282E-16, -20.00000000000000000, -5.000000000000000000 ) ) ;
#6520 = FACE_BOUND ( 'NONE', #3053, .T. ) ;
#6521 = CARTESIAN_POINT ( 'NONE',  ( 23.49999999999956657, -8.786575603324269439E-13, -13.00000000000000000 ) ) ;
#6522 = ADVANCED_FACE ( 'NONE', ( #84 ), #2404, .T. ) ;
#6523 = CARTESIAN_POINT ( 'NONE',  ( -4.606548227981508425, -6.456511556909257266, -7.591235721156635918 ) ) ;
#6524 = CARTESIAN_POINT ( 'NONE',  ( -6.874999999999997335, 4.690970937165711341, -7.298562697733101956 ) ) ;
#6525 = EDGE_CURVE ( 'NONE', #3803, #7205, #14785, .T. ) ;
#6526 = AXIS2_PLACEMENT_3D ( 'NONE', #3467, #13552, #8425 ) ;
#6527 = CARTESIAN_POINT ( 'NONE',  ( 4.795541693661363958, 1.415196051561583790, -5.000000000000000888 ) ) ;
#6528 = CARTESIAN_POINT ( 'NONE',  ( 0.5711823568785988625, 5.381735091635026613, -2.812500000000001776 ) ) ;
#6529 = VECTOR ( 'NONE', #14023, 1000.000000000000000 ) ;
#6530 = CARTESIAN_POINT ( 'NONE',  ( 2.071067811865462183, -29.18749999999999645, 5.000000000000013323 ) ) ;
#6531 = CARTESIAN_POINT ( 'NONE',  ( -1.846868145590734756, -24.12500000136559919, -4.458734125000000326 ) ) ;
#6532 = CARTESIAN_POINT ( 'NONE',  ( -4.799145180956616130, 0.5093500532425063732, -8.124999998634409692 ) ) ;
#6533 = ORIENTED_EDGE ( 'NONE', *, *, #10047, .F. ) ;
#6534 = LINE ( 'NONE', #14208, #14606 ) ;
#6535 = ORIENTED_EDGE ( 'NONE', *, *, #1236, .T. ) ;
#6536 = VERTEX_POINT ( 'NONE', #12112 ) ;
#6537 = CARTESIAN_POINT ( 'NONE',  ( 3.152801135295366208, -22.56250000136559564, 3.152801135295367985 ) ) ;
#6538 = DIRECTION ( 'NONE',  ( -0.000000000000000000, -1.000000000000000000, -0.000000000000000000 ) ) ;
#6539 = EDGE_LOOP ( 'NONE', ( #999, #14173, #254, #5326, #11140, #1636, #5148 ) ) ;
#6540 = DIRECTION ( 'NONE',  ( -0.000000000000000000, -1.000000000000000000, -0.000000000000000000 ) ) ;
#6541 = CONICAL_SURFACE ( 'NONE', #10917, 4.000000000000000000, 0.8911886515913786111 ) ;
#6542 = CARTESIAN_POINT ( 'NONE',  ( 7.264118654998711122, -4.945491722146229563, -7.907633014911222169 ) ) ;
#6543 = CARTESIAN_POINT ( 'NONE',  ( -3.033343224707664820, 3.753672977998667726, -0.9999999986344076941 ) ) ;
#6544 = PLANE ( 'NONE',  #8102 ) ;
#6545 =( BOUNDED_SURFACE ( )  B_SPLINE_SURFACE ( 3, 2, ( 
 ( #10681, #14399, #14549 ),
 ( #6975, #7130, #981 ),
 ( #15777, #9318, #8429 ),
 ( #11876, #5673, #5745 ),
 ( #14239, #3161, #8110 ),
 ( #3878, #12355, #173 ) ),
 .UNSPECIFIED., .F., .F., .F. ) 
 B_SPLINE_SURFACE_WITH_KNOTS ( ( 4, 2, 4 ),
 ( 3, 3 ),
 ( 0.02032853247518126225, 0.02278863295364821212, 0.02524873343211516200 ),
 ( 0.000000000000000000, 1.000000000000000000 ),
 .UNSPECIFIED. ) 
 GEOMETRIC_REPRESENTATION_ITEM ( )  RATIONAL_B_SPLINE_SURFACE ( (
 ( 1.000000000000000000, 0.8047781615896835161, 1.000000000000000000),
 ( 1.000000000000000000, 0.8123767586291043008, 1.000000000000000000),
 ( 1.000000000000000000, 0.8190662415562011134, 1.000000000000000000),
 ( 1.000000000000000000, 0.8192361015671398849, 1.000000000000000000),
 ( 1.000000000000000000, 0.8126135807102121689, 1.000000000000000000),
 ( 1.000000000000000000, 0.8047712338318585568, 1.000000000000000000) ) ) 
 REPRESENTATION_ITEM ( '' )  SURFACE ( )  );
#6546 = EDGE_CURVE ( 'NONE', #8765, #14249, #3554, .T. ) ;
#6547 = CARTESIAN_POINT ( 'NONE',  ( 5.000000000000000000, -28.00000000000000000, 0.000000000000000000 ) ) ;
#6548 = CARTESIAN_POINT ( 'NONE',  ( -4.211140560182196957, 2.431303136016537803, -3.745885042887433514 ) ) ;
#6549 = LINE ( 'NONE', #1608, #5106 ) ;
#6550 = CARTESIAN_POINT ( 'NONE',  ( -5.000000000000000888, -22.56250000273118772, 2.071067811865474617 ) ) ;
#6551 = B_SPLINE_CURVE_WITH_KNOTS ( 'NONE', 3,
 ( #6967, #14305, #9457, #4448, #11787, #6796, #10521, #508 ),
 .UNSPECIFIED., .F., .F.,
 ( 4, 2, 2, 4 ),
 ( 0.006061689441712458590, 0.007174127271521684238, 0.008286565101330909885, 0.01051144076094936118 ),
 .UNSPECIFIED. ) ;
#6552 = DIRECTION ( 'NONE',  ( 1.000000000000000000, 0.000000000000000000, 0.000000000000000000 ) ) ;
#6553 = CARTESIAN_POINT ( 'NONE',  ( -4.458734125000000326, -27.87500000136559564, 1.846868145590734089 ) ) ;
#6554 = CARTESIAN_POINT ( 'NONE',  ( -14.99999999999998934, -1.734723475976807094E-15, -9.999999999999998224 ) ) ;
#6555 = EDGE_LOOP ( 'NONE', ( #12250, #9807 ) ) ;
#6556 = ORIENTED_EDGE ( 'NONE', *, *, #12301, .T. ) ;
#6557 = EDGE_LOOP ( 'NONE', ( #1004, #5462 ) ) ;
#6558 = CARTESIAN_POINT ( 'NONE',  ( -44.36165667912468535, -3.982459619754737723, 20.27312360634764232 ) ) ;
#6559 = EDGE_LOOP ( 'NONE', ( #1620, #3316, #4306, #11275 ) ) ;
#6560 = LINE ( 'NONE', #9153, #8706 ) ;
#6561 = DIRECTION ( 'NONE',  ( 0.000000000000000000, 0.000000000000000000, 1.000000000000000000 ) ) ;
#6562 = ADVANCED_FACE ( 'NONE', ( #9777, #6229, #3706, #9929, #12352, #7209, #1048 ), #3791, .F. ) ;
#6563 = CARTESIAN_POINT ( 'NONE',  ( -4.209348295687703079, -3.401574460001763445, -4.312499997268815832 ) ) ;
#6564 = MECHANICAL_DESIGN_GEOMETRIC_PRESENTATION_REPRESENTATION (  '', ( #8382 ), #10938 ) ;
#6565 = CARTESIAN_POINT ( 'NONE',  ( 4.209348295687701302, 3.401574460001766109, -5.937500000000003553 ) ) ;
#6566 = AXIS2_PLACEMENT_3D ( 'NONE', #13220, #2159, #3450 ) ;
#6567 = CARTESIAN_POINT ( 'NONE',  ( 3.061616997868383141E-16, -31.75000000000000000, -5.000000000000000000 ) ) ;
#6568 = DIRECTION ( 'NONE',  ( -0.000000000000000000, 0.000000000000000000, -1.000000000000000000 ) ) ;
#6569 = ORIENTED_EDGE ( 'NONE', *, *, #6665, .T. ) ;
#6570 = ORIENTED_EDGE ( 'NONE', *, *, #6200, .T. ) ;
#6571 = CARTESIAN_POINT ( 'NONE',  ( 31.75426480542942898, -37.00000000000000711, -14.99999999999999645 ) ) ;
#6572 = CARTESIAN_POINT ( 'NONE',  ( 2.730187237215162345E-16, -31.18750000136559564, -4.458734124999999437 ) ) ;
#6573 = AXIS2_PLACEMENT_3D ( 'NONE', #13337, #6990, #5842 ) ;
#6574 = ORIENTED_EDGE ( 'NONE', *, *, #14920, .F. ) ;
#6575 = ITEM_DEFINED_TRANSFORMATION ( 'NONE', 'NONE', #13259,  #3223 ) ;
#6576 = CARTESIAN_POINT ( 'NONE',  ( -4.799145180956616130, 0.5093500532425063732, -7.124999998634407916 ) ) ;
#6577 = EDGE_CURVE ( 'NONE', #4817, #7310, #4926, .T. ) ;
#6578 = AXIS2_PLACEMENT_3D ( 'NONE', #12085, #15754, #14761 ) ;
#6579 = FACE_OUTER_BOUND ( 'NONE', #14060, .T. ) ;
#6580 = CIRCLE ( 'NONE', #7392, 2.499999999999999556 ) ;
#6581 = UNCERTAINTY_MEASURE_WITH_UNIT (LENGTH_MEASURE( 1.000000000000000082E-05 ), #9620, 'distance_accuracy_value', 'NONE');
#6582 = ADVANCED_BREP_SHAPE_REPRESENTATION ( '', ( #9475, #3223 ), #15373 ) ;
#6583 = AXIS2_PLACEMENT_3D ( 'NONE', #4701, #1063, #13333 ) ;
#6584 = CARTESIAN_POINT ( 'NONE',  ( -4.795541693661363958, -1.415196051561583790, -4.374999997268816720 ) ) ;
#6585 = SURFACE_SIDE_STYLE ('',( #4401 ) ) ;
#6586 = DIRECTION ( 'NONE',  ( 0.000000000000000000, 1.000000000000000000, 0.000000000000000000 ) ) ;
#6587 = ORIENTED_EDGE ( 'NONE', *, *, #1296, .T. ) ;
#6588 = VECTOR ( 'NONE', #8378, 1000.000000000000000 ) ;
#6589 = CYLINDRICAL_SURFACE ( 'NONE', #470, 3.499999999999999556 ) ;
#6590 = CARTESIAN_POINT ( 'NONE',  ( 0.5093500532425063732, 4.799145180956616130, -8.124999998634409692 ) ) ;
#6591 = CARTESIAN_POINT ( 'NONE',  ( 3.061616997868383141E-16, -26.87500000273118772, -5.000000000000000000 ) ) ;
#6592 = ORIENTED_EDGE ( 'NONE', *, *, #1796, .T. ) ;
#6593 = CARTESIAN_POINT ( 'NONE',  ( -35.00000000000000000, 40.00000000000000000, 6.000000000000000000 ) ) ;
#6594 = ORIENTED_EDGE ( 'NONE', *, *, #14209, .T. ) ;
#6595 = ORIENTED_EDGE ( 'NONE', *, *, #335, .F. ) ;
#6596 = CARTESIAN_POINT ( 'NONE',  ( -6.259644161404860030E-16, -4.618802153517027165, -3.433295621305388234 ) ) ;
#6597 = EDGE_CURVE ( 'NONE', #5167, #12864, #7453, .T. ) ;
#6598 = LINE ( 'NONE', #13036, #15410 ) ;
#6599 = ADVANCED_FACE ( 'NONE', ( #7125 ), #14868, .F. ) ;
#6600 = AXIS2_PLACEMENT_3D ( 'NONE', #11937, #1038, #8176 ) ;
#6601 = PLANE ( 'NONE',  #3214 ) ;
#6602 = AXIS2_PLACEMENT_3D ( 'NONE', #4125, #10198, #13977 ) ;
#6603 = FACE_OUTER_BOUND ( 'NONE', #5164, .T. ) ;
#6604 = CARTESIAN_POINT ( 'NONE',  ( -3.080866544137487395, -6.881514909249307088, -7.026396753507437865 ) ) ;
#6605 = DIRECTION ( 'NONE',  ( 0.000000000000000000, 1.000000000000000000, 0.000000000000000000 ) ) ;
#6606 = CARTESIAN_POINT ( 'NONE',  ( -4.391654775818395251, 2.390265326283148806, -6.625000000000002665 ) ) ;
#6607 = DIRECTION ( 'NONE',  ( -0.000000000000000000, -1.000000000000000000, -0.000000000000000000 ) ) ;
#6608 = CARTESIAN_POINT ( 'NONE',  ( -1.287237434361707233, -3.875615274277397937, -3.430618716626816500 ) ) ;
#6609 = DIRECTION ( 'NONE',  ( -0.000000000000000000, 1.000000000000000000, -0.000000000000000000 ) ) ;
#6610 = CARTESIAN_POINT ( 'NONE',  ( 2.131511515620586383, 3.916244202832140253, -7.437499998634407916 ) ) ;
#6611 = ORIENTED_EDGE ( 'NONE', *, *, #8695, .F. ) ;
#6612 = AXIS2_PLACEMENT_3D ( 'NONE', #6853, #3511, #11762 ) ;
#6613 = UNCERTAINTY_MEASURE_WITH_UNIT (LENGTH_MEASURE( 1.000000000000000082E-05 ), #4813, 'distance_accuracy_value', 'NONE');
#6614 = CARTESIAN_POINT ( 'NONE',  ( 7.500000000000003553, -4.330127018922199866, -7.422398894150035176 ) ) ;
#6615 = ORIENTED_EDGE ( 'NONE', *, *, #2752, .T. ) ;
#6616 = ORIENTED_EDGE ( 'NONE', *, *, #12795, .F. ) ;
#6617 = AXIS2_PLACEMENT_3D ( 'NONE', #12083, #12236, #14597 ) ;
#6618 =( REPRESENTATION_RELATIONSHIP ('NONE','NONE', #4176, #4696 ) REPRESENTATION_RELATIONSHIP_WITH_TRANSFORMATION ( #14908 )SHAPE_REPRESENTATION_RELATIONSHIP( ) );
#6619 = CARTESIAN_POINT ( 'NONE',  ( -1.846868145590734756, -31.37500000136559564, -4.458734125000000326 ) ) ;
#6620 = ADVANCED_FACE ( 'NONE', ( #3466 ), #1765, .T. ) ;
#6621 = DIRECTION ( 'NONE',  ( -0.000000000000000000, -0.000000000000000000, 1.000000000000000000 ) ) ;
#6622 = ADVANCED_FACE ( 'NONE', ( #15848 ), #2256, .T. ) ;
#6623 = ORIENTED_EDGE ( 'NONE', *, *, #3033, .F. ) ;
#6624 = DIRECTION ( 'NONE',  ( -0.000000000000000000, -1.000000000000000000, -0.000000000000000000 ) ) ;
#6625 = COLOUR_RGB ( '', 0.09019608, 0.27058824, 0.51372549) ;
#6626 = DIRECTION ( 'NONE',  ( 0.000000000000000000, -1.000000000000000000, 0.000000000000000000 ) ) ;
#6627 = CARTESIAN_POINT ( 'NONE',  ( 3.916244202832140253, -2.131511515620588160, -2.437499998634407028 ) ) ;
#6628 = DIRECTION ( 'NONE',  ( -0.000000000000000000, 1.000000000000000000, -0.000000000000000000 ) ) ;
#6629 = CARTESIAN_POINT ( 'NONE',  ( -2.071067811865475061, -27.68750000000000355, -5.000000000000000888 ) ) ;
#6630 = CLOSED_SHELL ( 'NONE', ( #8288, #2170, #10775, #5653, #7709, #15881, #12195, #1313, #12636, #2773, #10449, #2277, #13212, #1076, #3537, #10545 ) ) ;
#6631 = CARTESIAN_POINT ( 'NONE',  ( 3.916244202832140253, -2.131511515620588160, -5.437499998634406140 ) ) ;
#6632 = CARTESIAN_POINT ( 'NONE',  ( 4.000000000000000000, 2.309401076758497151, -5.000000000000000000 ) ) ;
#6633 = DIRECTION ( 'NONE',  ( 0.000000000000000000, 0.000000000000000000, 1.000000000000000000 ) ) ;
#6634 = CARTESIAN_POINT ( 'NONE',  ( -9.184850993605147944E-16, -25.37500000273118417, 5.000000000000000000 ) ) ;
#6635 = LINE ( 'NONE', #13896, #12964 ) ;
#6636 = CARTESIAN_POINT ( 'NONE',  ( 2.730187237215162345E-16, -28.18750000136559564, -4.458734124999999437 ) ) ;
#6637 = CARTESIAN_POINT ( 'NONE',  ( -60.00000000000000000, 88.59290746114278647, 17.99999999999999289 ) ) ;
#6638 = ORIENTED_EDGE ( 'NONE', *, *, #250, .T. ) ;
#6639 = VECTOR ( 'NONE', #313, 1000.000000000000000 ) ;
#6640 = EDGE_LOOP ( 'NONE', ( #14553, #9288, #5104, #6704 ) ) ;
#6641 = PRODUCT_DEFINITION_SHAPE ( 'NONE', 'NONE',  #15982 ) ;
#6643 = EDGE_CURVE ( 'NONE', #15626, #3401, #10171, .T. ) ;
#6642 = ORIENTED_EDGE ( 'NONE', *, *, #205, .T. ) ;
#6644 = CARTESIAN_POINT ( 'NONE',  ( 5.200000000000002842, 0.000000000000000000, 0.000000000000000000 ) ) ;
#6645 = EDGE_CURVE ( 'NONE', #11474, #8700, #8504, .T. ) ;
#6646 = CIRCLE ( 'NONE', #14894, 7.500000000000001776 ) ;
#6647 = EDGE_CURVE ( 'NONE', #678, #7875, #10375, .T. ) ;
#6648 = ORIENTED_EDGE ( 'NONE', *, *, #2916, .T. ) ;
#6649 = CYLINDRICAL_SURFACE ( 'NONE', #7162, 2.649999999999992806 ) ;
#6650 =( BOUNDED_CURVE ( )  B_SPLINE_CURVE ( 2, ( #9277, #14200, #3123, #8067, #704, #5629, #10574, #15499, #4649 ),
 .UNSPECIFIED., .F., .F. ) 
 B_SPLINE_CURVE_WITH_KNOTS ( ( 3, 2, 2, 2, 3 ),
 ( 0.6249999999999998890, 0.6374999999999998446, 0.6499999999999999112, 0.6624999999999998668, 0.6749999999999999334 ),
 .UNSPECIFIED. ) 
 CURVE ( )  GEOMETRIC_REPRESENTATION_ITEM ( )  RATIONAL_B_SPLINE_CURVE ( ( 1.000000000000000666, 0.9238795325112860723, 1.000000000000000000, 0.9238795325112867385, 1.000000000000000000, 0.9238795325112867385, 1.000000000000000000, 0.9238795325112874046, 0.9999999999999993339 ) ) 
 REPRESENTATION_ITEM ( '' )  );
#6651 = AXIS2_PLACEMENT_3D ( 'NONE', #6506, #11264, #6189 ) ;
#6652 = LINE ( 'NONE', #8997, #15308 ) ;
#6653 = CARTESIAN_POINT ( 'NONE',  ( -3.152801135295367985, -30.06250000136559564, 3.152801135295367096 ) ) ;
#6654 = CARTESIAN_POINT ( 'NONE',  ( -4.999999999999844569, 1.272547481429019856, -6.461597479913464781 ) ) ;
#6655 = ITEM_DEFINED_TRANSFORMATION ( 'NONE', 'NONE', #1401,  #3223 ) ;
#6656 = CARTESIAN_POINT ( 'NONE',  ( 9.999999999999891642, -20.00000000000000000, -17.32050807568883499 ) ) ;
#6657 = CARTESIAN_POINT ( 'NONE',  ( -1.261996585732579224, 4.276409079477648589, -0.3124999986344085823 ) ) ;
#6658 = ORIENTED_EDGE ( 'NONE', *, *, #1796, .F. ) ;
#6659 =( NAMED_UNIT ( * ) PLANE_ANGLE_UNIT ( ) SI_UNIT ( $, .RADIAN. ) );
#6660 = VECTOR ( 'NONE', #6789, 1000.000000000000000 ) ;
#6661 = VERTEX_POINT ( 'NONE', #1204 ) ;
#6662 = DIRECTION ( 'NONE',  ( -0.7071067811865369146, 8.659560562355062281E-17, -0.7071067811865582309 ) ) ;
#6663 = CIRCLE ( 'NONE', #11546, 2.499999999999998668 ) ;
#6664 = CARTESIAN_POINT ( 'NONE',  ( 3.152801135295366208, -27.56250000136559564, 3.152801135295367985 ) ) ;
#6665 = EDGE_CURVE ( 'NONE', #15230, #15294, #13466, .T. ) ;
#6666 = VERTEX_POINT ( 'NONE', #4189 ) ;
#6667 = VECTOR ( 'NONE', #8942, 1000.000000000000227 ) ;
#6668 = PLANE ( 'NONE',  #12255 ) ;
#6669 = FACE_OUTER_BOUND ( 'NONE', #13874, .T. ) ;
#6670 = AXIS2_PLACEMENT_3D ( 'NONE', #6849, #11679, #709 ) ;
#6671 = EDGE_CURVE ( 'NONE', #9599, #6256, #7773, .T. ) ;
#6672 = DIRECTION ( 'NONE',  ( -0.000000000000000000, -0.000000000000000000, -1.000000000000000000 ) ) ;
#6673 = VECTOR ( 'NONE', #1734, 1000.000000000000000 ) ;
#6674 = CARTESIAN_POINT ( 'NONE',  ( -3.753672977998669946, -3.033343224707661712, 1.000000001365594082 ) ) ;
#6675 = DIRECTION ( 'NONE',  ( -0.000000000000000000, 1.000000000000000000, -0.000000000000000000 ) ) ;
#6676 = EDGE_CURVE ( 'NONE', #2119, #3645, #2516, .T. ) ;
#6677 = PLANE ( 'NONE',  #8243 ) ;
#6678 = CARTESIAN_POINT ( 'NONE',  ( -4.458734124999999437, -23.25000000136559564, -1.846868145590735644 ) ) ;
#6679 = EDGE_LOOP ( 'NONE', ( #4021, #6052, #3290 ) ) ;
#6680 = PLANE ( 'NONE',  #6921 ) ;
#6681 = FACE_OUTER_BOUND ( 'NONE', #14537, .T. ) ;
#6682 = AXIS2_PLACEMENT_3D ( 'NONE', #358, #1308, #8840 ) ;
#6683 = CARTESIAN_POINT ( 'NONE',  ( -2.071067811865482167, -26.81250000273118417, -4.999999999999992895 ) ) ;
#6684 = ORIENTED_EDGE ( 'NONE', *, *, #888, .T. ) ;
#6685 = DIRECTION ( 'NONE',  ( 0.000000000000000000, 0.000000000000000000, 1.000000000000000000 ) ) ;
#6686 = ORIENTED_EDGE ( 'NONE', *, *, #1206, .T. ) ;
#6687 = EDGE_LOOP ( 'NONE', ( #10153, #13602, #7741, #4694 ) ) ;
#6688 = CARTESIAN_POINT ( 'NONE',  ( 4.391654775818395251, -2.390265326283149694, -0.1250000000000035805 ) ) ;
#6689 = CARTESIAN_POINT ( 'NONE',  ( -2.807080416178626692, 3.225969019225154444, -3.502507215260441065 ) ) ;
#6690 = VECTOR ( 'NONE', #7669, 1000.000000000000000 ) ;
#6691 = CARTESIAN_POINT ( 'NONE',  ( -116.3391301858327012, -120.2076149402627010, -13.35786437626904721 ) ) ;
#6692 = CIRCLE ( 'NONE', #14175, 0.5155456020628804703 ) ;
#6693 = FACE_OUTER_BOUND ( 'NONE', #1930, .T. ) ;
#6694 = CARTESIAN_POINT ( 'NONE',  ( -81.33974596215558961, -99.99999999999995737, 17.50000000000000000 ) ) ;
#6695 = DIRECTION ( 'NONE',  ( 0.000000000000000000, 0.000000000000000000, 1.000000000000000000 ) ) ;
#6696 = CYLINDRICAL_SURFACE ( 'NONE', #2133, 10.00000000000000000 ) ;
#6697 = ADVANCED_FACE ( 'NONE', ( #12741 ), #1443, .F. ) ;
#6698 = CONICAL_SURFACE ( 'NONE', #12829, 2.041999999999999815, 1.047197551196591858 ) ;
#6699 = CARTESIAN_POINT ( 'NONE',  ( 24.55500000000002103, 0.000000000000000000, 0.000000000000000000 ) ) ;
#6700 = EDGE_CURVE ( 'NONE', #10386, #11169, #6358, .T. ) ;
#6701 = CARTESIAN_POINT ( 'NONE',  ( 2.730187237215162345E-16, -23.18750000136559564, -4.458734124999999437 ) ) ;
#6702 = AXIS2_PLACEMENT_3D ( 'NONE', #11940, #1195, #12019 ) ;
#6703 = CARTESIAN_POINT ( 'NONE',  ( 0.5093500532425063732, 4.799145180956616130, -7.374999998634408804 ) ) ;
#6704 = ORIENTED_EDGE ( 'NONE', *, *, #2866, .F. ) ;
#6705 = CARTESIAN_POINT ( 'NONE',  ( 1.249999999999999556, 7.938566201357357244, -7.198902722707428481 ) ) ;
#6706 = ORIENTED_EDGE ( 'NONE', *, *, #6933, .T. ) ;
#6707 = VERTEX_POINT ( 'NONE', #4888 ) ;
#6708 = VERTEX_POINT ( 'NONE', #15884 ) ;
#6709 = CARTESIAN_POINT ( 'NONE',  ( -8.190561711645485556E-16, -30.93750000136559564, 4.458734124999999437 ) ) ;
#6710 = DIRECTION ( 'NONE',  ( 0.000000000000000000, 0.000000000000000000, 1.000000000000000000 ) ) ;
#6711 = VERTEX_POINT ( 'NONE', #44 ) ;
#6712 = FACE_OUTER_BOUND ( 'NONE', #13055, .T. ) ;
#6713 = CIRCLE ( 'NONE', #3820, 5.000000000000001776 ) ;
#6714 = CARTESIAN_POINT ( 'NONE',  ( 19.99999999999956657, -8.786575603324269439E-13, -4.500000000000000000 ) ) ;
#6715 = CARTESIAN_POINT ( 'NONE',  ( 3.033343224707661712, -3.753672977998669502, -5.499999998634407916 ) ) ;
#6716 = CARTESIAN_POINT ( 'NONE',  ( 0.8467517840721383582, 4.385914846095951170, -0.3789984458506778786 ) ) ;
#6717 = CARTESIAN_POINT ( 'NONE',  ( 5.000000000000000888, -25.93750000000000355, -2.071067811865475505 ) ) ;
#6718 = CARTESIAN_POINT ( 'NONE',  ( 3.753672977998667726, 3.033343224707664376, -5.249999998634407028 ) ) ;
#6719 = DIRECTION ( 'NONE',  ( -1.239088197126290570E-16, 0.000000000000000000, -1.000000000000000000 ) ) ;
#6720 = CARTESIAN_POINT ( 'NONE',  ( 35.00000000000000000, 37.00000000000000000, -2.650000000000001243 ) ) ;
#6721 = EDGE_CURVE ( 'NONE', #349, #12690, #3830, .T. ) ;
#6722 = CARTESIAN_POINT ( 'NONE',  ( -5.000000000000000888, -24.56250000273118772, 2.071067811865474617 ) ) ;
#6723 = PRODUCT_DEFINITION ( 'UNKNOWN', '', #8973, #3833 ) ;
#6724 = FACE_OUTER_BOUND ( 'NONE', #6500, .T. ) ;
#6725 = CARTESIAN_POINT ( 'NONE',  ( 3.152801135295366208, -24.56250000136559564, 3.152801135295367985 ) ) ;
#6726 = CARTESIAN_POINT ( 'NONE',  ( -9.184850993605147944E-16, -22.37500000273118417, 5.000000000000000000 ) ) ;
#6727 = ORIENTED_EDGE ( 'NONE', *, *, #1950, .F. ) ;
#6728 = ORIENTED_EDGE ( 'NONE', *, *, #800, .F. ) ;
#6729 = CARTESIAN_POINT ( 'NONE',  ( 39.53738644056090124, -3.000000000000000000, 28.48076211354432985 ) ) ;
#6730 = VERTEX_POINT ( 'NONE', #2609 ) ;
#6731 = CARTESIAN_POINT ( 'NONE',  ( -5.000000000000092371, -0.7223674278660636716, -7.396799362785970722 ) ) ;
#6732 = ORIENTED_EDGE ( 'NONE', *, *, #1399, .T. ) ;
#6733 = CARTESIAN_POINT ( 'NONE',  ( 4.000000000000000000, 2.309401076758497151, -5.000000000000000000 ) ) ;
#6734 = CARTESIAN_POINT ( 'NONE',  ( 6.123233995736766282E-16, -20.00000000000000000, 5.000000000000000000 ) ) ;
#6735 = CARTESIAN_POINT ( 'NONE',  ( -4.458734125000001214, -26.12500000136559919, 1.846868145590734089 ) ) ;
#6736 = CARTESIAN_POINT ( 'NONE',  ( -4.999999999999844569, 1.272547481429019856, -5.586597482644649837 ) ) ;
#6737 = EDGE_CURVE ( 'NONE', #11376, #11740, #3038, .T. ) ;
#6738 = EDGE_CURVE ( 'NONE', #14678, #13455, #12341, .T. ) ;
#6739 = DIRECTION ( 'NONE',  ( -0.000000000000000000, 1.000000000000000000, -0.000000000000000000 ) ) ;
#6740 = EDGE_CURVE ( 'NONE', #10519, #9186, #6692, .T. ) ;
#6741 = DIRECTION ( 'NONE',  ( -0.000000000000000000, -0.000000000000000000, -1.000000000000000000 ) ) ;
#6742 = CARTESIAN_POINT ( 'NONE',  ( -0.5093500532425060401, -4.799145180956616130, 0.1250000013655913900 ) ) ;
#6743 = ORIENTED_EDGE ( 'NONE', *, *, #5593, .F. ) ;
#6744 = VERTEX_POINT ( 'NONE', #1158 ) ;
#6745 = LINE ( 'NONE', #13918, #10582 ) ;
#6746 = ORIENTED_EDGE ( 'NONE', *, *, #1574, .T. ) ;
#6747 = DIRECTION ( 'NONE',  ( 0.000000000000000000, 1.000000000000000000, 0.000000000000000000 ) ) ;
#6748 = CARTESIAN_POINT ( 'NONE',  ( 1.415196051561583790, -4.795541693661363958, -3.124999997268815832 ) ) ;
#6749 = CARTESIAN_POINT ( 'NONE',  ( -0.5711823568785977523, -5.381735091635034607, -8.187499997268814056 ) ) ;
#6750 = EDGE_CURVE ( 'NONE', #8728, #15000, #1294, .T. ) ;
#6751 = CARTESIAN_POINT ( 'NONE',  ( -5.381735091635034607, 0.5711823568785950878, -7.437499997268817609 ) ) ;
#6752 = CARTESIAN_POINT ( 'NONE',  ( -81.33974596215560382, -110.0591436588189538, 17.50000000000000000 ) ) ;
#6753 = DIRECTION ( 'NONE',  ( -1.000000000000000000, 0.000000000000000000, -0.000000000000000000 ) ) ;
#6754 = CARTESIAN_POINT ( 'NONE',  ( -31.74999999999995737, 0.000000000000000000, 0.000000000000000000 ) ) ;
#6755 = VERTEX_POINT ( 'NONE', #8538 ) ;
#6756 = DIRECTION ( 'NONE',  ( 0.000000000000000000, 0.000000000000000000, -1.000000000000000000 ) ) ;
#6757 = DIRECTION ( 'NONE',  ( -0.8660254037844383745, -0.5000000000000004441, 0.000000000000000000 ) ) ;
#6758 = DIRECTION ( 'NONE',  ( 0.000000000000000000, -1.000000000000000000, 0.000000000000000000 ) ) ;
#6759 = VERTEX_POINT ( 'NONE', #13428 ) ;
#6760 = CARTESIAN_POINT ( 'NONE',  ( -4.197312064133472020, -0.8182229787990021874, -3.502518405183886685 ) ) ;
#6761 = VERTEX_POINT ( 'NONE', #13591 ) ;
#6762 = ORIENTED_EDGE ( 'NONE', *, *, #3515, .T. ) ;
#6763 = DIRECTION ( 'NONE',  ( -0.000000000000000000, 1.000000000000000000, -0.000000000000000000 ) ) ;
#6764 = DIRECTION ( 'NONE',  ( -0.000000000000000000, -1.000000000000000000, -0.000000000000000000 ) ) ;
#6765 = DIRECTION ( 'NONE',  ( 0.000000000000000000, 0.000000000000000000, 1.000000000000000000 ) ) ;
#6766 = CARTESIAN_POINT ( 'NONE',  ( 5.000000000000002665, 1.275685995473128912E-14, -5.045263047592944083 ) ) ;
#6767 = DIRECTION ( 'NONE',  ( 1.000000000000000000, 0.000000000000000000, 0.000000000000000000 ) ) ;
#6768 = FACE_OUTER_BOUND ( 'NONE', #5456, .T. ) ;
#6769 = CARTESIAN_POINT ( 'NONE',  ( -21.01110699893041556, 2.000000000000000000, -33.74230484541335073 ) ) ;
#6770 = CARTESIAN_POINT ( 'NONE',  ( -36.99999999999999289, -13.00000000000000178, -1.999999999999170885 ) ) ;
#6771 = DIRECTION ( 'NONE',  ( 0.000000000000000000, 0.000000000000000000, -1.000000000000000000 ) ) ;
#6772 = CARTESIAN_POINT ( 'NONE',  ( -4.458734125000000326, -22.00000000136559208, -1.846868145590735644 ) ) ;
#6773 = CARTESIAN_POINT ( 'NONE',  ( -3.916244202832140253, 2.131511515620587272, 0.06250000136559172303 ) ) ;
#6774 = EDGE_LOOP ( 'NONE', ( #14083, #2920, #5199 ) ) ;
#6775 = FACE_OUTER_BOUND ( 'NONE', #8649, .T. ) ;
#6776 = ORIENTED_EDGE ( 'NONE', *, *, #6147, .T. ) ;
#6777 = ORIENTED_EDGE ( 'NONE', *, *, #2731, .T. ) ;
#6778 = CARTESIAN_POINT ( 'NONE',  ( 1.846868145590736310, -22.62500000136559564, 4.458734124999999437 ) ) ;
#6779 = VERTEX_POINT ( 'NONE', #11029 ) ;
#6780 = CARTESIAN_POINT ( 'NONE',  ( 0.000000000000000000, 0.000000000000000000, -0.5776712190230133270 ) ) ;
#6781 = ADVANCED_FACE ( 'NONE', ( #9887 ), #2368, .F. ) ;
#6782 = DIRECTION ( 'NONE',  ( 0.000000000000000000, 0.000000000000000000, 1.000000000000000000 ) ) ;
#6783 = AXIS2_PLACEMENT_3D ( 'NONE', #6210, #2387, #9907 ) ;
#6784 = CARTESIAN_POINT ( 'NONE',  ( -2.131511515620587272, -3.916244202832140253, -5.687499998634406140 ) ) ;
#6785 = CARTESIAN_POINT ( 'NONE',  ( 1.567478505476135000E-15, 4.618802153517012954, -3.504269196027527844 ) ) ;
#6786 = CARTESIAN_POINT ( 'NONE',  ( -5.000000000000000000, -24.50000000000000000, -6.123233995736766282E-16 ) ) ;
#6787 = CARTESIAN_POINT ( 'NONE',  ( -4.276409079477644148, -1.261996585732578335, -7.812499998634407916 ) ) ;
#6788 = DIRECTION ( 'NONE',  ( 0.000000000000000000, 0.000000000000000000, 1.000000000000000000 ) ) ;
#6789 = DIRECTION ( 'NONE',  ( 0.000000000000000000, -1.000000000000000000, 0.000000000000000000 ) ) ;
#6790 = CARTESIAN_POINT ( 'NONE',  ( -3.535533905932737309, -23.75000000273118772, -3.535533905932738197 ) ) ;
#6791 = VERTEX_POINT ( 'NONE', #12217 ) ;
#6792 = CARTESIAN_POINT ( 'NONE',  ( 4.458734124999999437, -28.37500000136559564, -1.846868145590734978 ) ) ;
#6793 = CARTESIAN_POINT ( 'NONE',  ( -34.99999999999999289, -13.00000000000000178, 2.000000000000830447 ) ) ;
#6794 = ORIENTED_EDGE ( 'NONE', *, *, #8418, .F. ) ;
#6795 = ORIENTED_EDGE ( 'NONE', *, *, #8718, .T. ) ;
#6796 = CARTESIAN_POINT ( 'NONE',  ( 7.500000000000000000, -1.486698507076799070, -0.09861472150523925562 ) ) ;
#6797 = VECTOR ( 'NONE', #4766, 1000.000000000000000 ) ;
#6798 = CIRCLE ( 'NONE', #6016, 2.649999999999985700 ) ;
#6799 = DIRECTION ( 'NONE',  ( 0.000000000000000000, 0.000000000000000000, 1.000000000000000000 ) ) ;
#6800 = VERTEX_POINT ( 'NONE', #11106 ) ;
#6801 = CARTESIAN_POINT ( 'NONE',  ( -9.184850993605147944E-16, -24.37500000273118772, 5.000000000000000000 ) ) ;
#6802 = EDGE_CURVE ( 'NONE', #15426, #15784, #3326, .T. ) ;
#6803 = ADVANCED_FACE ( 'NONE', ( #6263 ), #9972, .F. ) ;
#6804 = PRODUCT_DEFINITION_SHAPE ( 'NONE', 'NONE',  #5020 ) ;
#6805 = CARTESIAN_POINT ( 'NONE',  ( 39.53738644055563611, -4.730053418719265323, -28.48076211352709564 ) ) ;
#6806 = CARTESIAN_POINT ( 'NONE',  ( 1.846868145590735200, -29.50000000136559564, -4.458734125000000326 ) ) ;
#6807 = LINE ( 'NONE', #9157, #7545 ) ;
#6808 = DIRECTION ( 'NONE',  ( -0.000000000000000000, -1.000000000000000000, -0.000000000000000000 ) ) ;
#6809 = CARTESIAN_POINT ( 'NONE',  ( 4.795541693661363958, 1.415196051561583790, -7.874999997268816720 ) ) ;
#6810 = CARTESIAN_POINT ( 'NONE',  ( 4.276409079477644148, 1.261996585732577891, 1.437500001365592972 ) ) ;
#6811 = ORIENTED_EDGE ( 'NONE', *, *, #4602, .F. ) ;
#6812 =( NAMED_UNIT ( * ) PLANE_ANGLE_UNIT ( ) SI_UNIT ( $, .RADIAN. ) );
#6813 = ORIENTED_EDGE ( 'NONE', *, *, #12208, .T. ) ;
#6814 = DIRECTION ( 'NONE',  ( 0.4999999999999998335, -0.000000000000000000, 0.8660254037844387076 ) ) ;
#6815 = ORIENTED_EDGE ( 'NONE', *, *, #9985, .T. ) ;
#6816 = ITEM_DEFINED_TRANSFORMATION ( 'NONE', 'NONE', #4246,  #3223 ) ;
#6817 = EDGE_CURVE ( 'NONE', #1886, #658, #15464, .T. ) ;
#6818 = AXIS2_PLACEMENT_3D ( 'NONE', #11423, #10068, #370 ) ;
#6819 = EDGE_CURVE ( 'NONE', #13728, #4594, #13238, .T. ) ;
#6820 = CARTESIAN_POINT ( 'NONE',  ( -99.99999999999998579, -100.7735026918962831, -17.50000000000000000 ) ) ;
#6821 = DIRECTION ( 'NONE',  ( 0.000000000000000000, 0.000000000000000000, 1.000000000000000000 ) ) ;
#6822 = CARTESIAN_POINT ( 'NONE',  ( 5.000000000000004441, -2.247904837838113790E-16, -7.920263044861759028 ) ) ;
#6823 = CARTESIAN_POINT ( 'NONE',  ( 5.381735091635035495, -0.5711823568785978633, -5.937499997268815832 ) ) ;
#6824 = CARTESIAN_POINT ( 'NONE',  ( 5.000000000000091482, 0.7223674278660682235, -1.021799365517154223 ) ) ;
#6825 =( NAMED_UNIT ( * ) SI_UNIT ( $, .STERADIAN. ) SOLID_ANGLE_UNIT ( ) );
#6826 = DIRECTION ( 'NONE',  ( 1.000000000000000000, 0.000000000000000000, 0.000000000000000000 ) ) ;
#6827 = ORIENTED_EDGE ( 'NONE', *, *, #3719, .T. ) ;
#6828 = CARTESIAN_POINT ( 'NONE',  ( 2.500000000000000000, 2.357898499370433054, -1.951563910473907981E-15 ) ) ;
#6829 = FACE_OUTER_BOUND ( 'NONE', #9619, .T. ) ;
#6830 =( NAMED_UNIT ( * ) PLANE_ANGLE_UNIT ( ) SI_UNIT ( $, .RADIAN. ) );
#6831 = ORIENTED_EDGE ( 'NONE', *, *, #9501, .F. ) ;
#6832 = LINE ( 'NONE', #14497, #5411 ) ;
#6833 = ORIENTED_EDGE ( 'NONE', *, *, #2350, .T. ) ;
#6834 = AXIS2_PLACEMENT_3D ( 'NONE', #11926, #1836, #1915 ) ;
#6835 = VECTOR ( 'NONE', #12, 1000.000000000000000 ) ;
#6836 = EDGE_LOOP ( 'NONE', ( #4349, #1393, #302, #9070, #7746 ) ) ;
#6837 = DIRECTION ( 'NONE',  ( -1.000000000000000000, 0.000000000000000000, 0.000000000000000000 ) ) ;
#6838 = ADVANCED_FACE ( 'NONE', ( #6579 ), #2288, .T. ) ;
#6839 = CYLINDRICAL_SURFACE ( 'NONE', #12798, 5.000000000000000000 ) ;
#6840 = EDGE_CURVE ( 'NONE', #13973, #3228, #503, .T. ) ;
#6841 = CARTESIAN_POINT ( 'NONE',  ( -36.99999999999999289, -11.00000000000000178, 2.000000000000830891 ) ) ;
#6842 = AXIS2_PLACEMENT_3D ( 'NONE', #15867, #2280, #1143 ) ;
#6843 = DIRECTION ( 'NONE',  ( 0.000000000000000000, -1.000000000000000000, 0.000000000000000000 ) ) ;
#6844 = DIRECTION ( 'NONE',  ( 0.000000000000000000, -0.000000000000000000, 1.000000000000000000 ) ) ;
#6845 = MECHANICAL_DESIGN_GEOMETRIC_PRESENTATION_REPRESENTATION (  '', ( #7352 ), #144 ) ;
#6846 = CARTESIAN_POINT ( 'NONE',  ( -7.500000000000000000, -4.330127018922196314, -7.422398894150035176 ) ) ;
#6847 = CARTESIAN_POINT ( 'NONE',  ( 6.293430271071538407, -5.026740376715105540, -0.4524126574264555334 ) ) ;
#6848 = CARTESIAN_POINT ( 'NONE',  ( 79.38739406438118351, 1.999999999999998224, 12.50099999999964417 ) ) ;
#6849 = CARTESIAN_POINT ( 'NONE',  ( 0.000000000000000000, 0.000000000000000000, 0.000000000000000000 ) ) ;
#6850 = CARTESIAN_POINT ( 'NONE',  ( 3.152801135295367541, -28.56250000136559564, -3.152801135295367541 ) ) ;
#6851 = CARTESIAN_POINT ( 'NONE',  ( 2.131511515620586383, 3.916244202832140253, 0.8125000013655924169 ) ) ;
#6852 = ORIENTED_EDGE ( 'NONE', *, *, #14294, .F. ) ;
#6853 = CARTESIAN_POINT ( 'NONE',  ( -21.01110699893060030, -3.000000000000001332, 36.39230484541324273 ) ) ;
#6854 = ORIENTED_EDGE ( 'NONE', *, *, #7307, .T. ) ;
#6855 = ORIENTED_EDGE ( 'NONE', *, *, #7326, .F. ) ;
#6856 = COLOUR_RGB ( '', 0.09019608, 0.27058824, 0.51372549) ;
#6857 = B_SPLINE_CURVE_WITH_KNOTS ( 'NONE', 3,
 ( #12722, #12404, #1339, #147, #12647, #5066, #1586, #6524, #12481 ),
 .UNSPECIFIED., .F., .F.,
 ( 4, 2, 1, 2, 4 ),
 ( 0.000000000000000000, 0.002165063509461100100, 0.004330127018922199332, 0.006495190528383298564, 0.008660254037844396929 ),
 .UNSPECIFIED. ) ;
#6859 = AXIS2_PLACEMENT_3D ( 'NONE', #3022, #13852, #10385 ) ;
#6858 = SURFACE_STYLE_USAGE ( .BOTH. , #1912 ) ;
#6860 = CARTESIAN_POINT ( 'NONE',  ( -4.458734125000000326, -25.25000000136559564, -1.846868145590735644 ) ) ;
#6861 = CARTESIAN_POINT ( 'NONE',  ( 2.345747346278113987, -3.264484291692503870, -0.01223254789874484924 ) ) ;
#6862 = AXIS2_PLACEMENT_3D ( 'NONE', #11494, #15552, #10620 ) ;
#6863 = EDGE_CURVE ( 'NONE', #2882, #4597, #7880, .T. ) ;
#6864 = DIRECTION ( 'NONE',  ( -0.000000000000000000, 1.000000000000000000, -0.000000000000000000 ) ) ;
#6865 = DIRECTION ( 'NONE',  ( -1.000000000000000000, -0.000000000000000000, -0.000000000000000000 ) ) ;
#6866 = CARTESIAN_POINT ( 'NONE',  ( -4.799145180956616130, 0.5093500532425063732, -6.874999998634407916 ) ) ;
#6867 = DIRECTION ( 'NONE',  ( -0.000000000000000000, 1.000000000000000000, -0.000000000000000000 ) ) ;
#6868 = CARTESIAN_POINT ( 'NONE',  ( -3.535533905932737309, -24.62500000000000000, -3.535533905932738197 ) ) ;
#6869 = AXIS2_PLACEMENT_3D ( 'NONE', #7114, #13157, #2091 ) ;
#6870 = CARTESIAN_POINT ( 'NONE',  ( 1.415196051561583790, -4.795541693661363958, 1.749999999999998002 ) ) ;
#6871 = FACE_OUTER_BOUND ( 'NONE', #12582, .T. ) ;
#6872 = CARTESIAN_POINT ( 'NONE',  ( 19.99999999999956657, -8.786575603324269439E-13, -4.500000000000000000 ) ) ;
#6873 = CARTESIAN_POINT ( 'NONE',  ( -5.000000000000000888, -21.68750000273119127, -2.071067811865475949 ) ) ;
#6874 = AXIS2_PLACEMENT_3D ( 'NONE', #3390, #15842, #3702 ) ;
#6875 = ORIENTED_EDGE ( 'NONE', *, *, #10758, .F. ) ;
#6876 = CIRCLE ( 'NONE', #1956, 2.055000000000000160 ) ;
#6877 = CARTESIAN_POINT ( 'NONE',  ( 2.730187237215162345E-16, -27.18750000136559564, -4.458734124999999437 ) ) ;
#6878 = EDGE_CURVE ( 'NONE', #1232, #10374, #1720, .T. ) ;
#6879 = PLANE ( 'NONE',  #14856 ) ;
#6880 = ORIENTED_EDGE ( 'NONE', *, *, #10177, .T. ) ;
#6881 = ORIENTED_EDGE ( 'NONE', *, *, #953, .F. ) ;
#6882 = LINE ( 'NONE', #10605, #5130 ) ;
#6883 = CARTESIAN_POINT ( 'NONE',  ( -2.390265326283148806, -4.391654775818394363, -7.249999997268815832 ) ) ;
#6884 =( BOUNDED_CURVE ( )  B_SPLINE_CURVE ( 2, ( #7122, #12024, #8185, #1937, #15609, #898, #818, #973, #6801 ),
 .UNSPECIFIED., .F., .F. ) 
 B_SPLINE_CURVE_WITH_KNOTS ( ( 3, 2, 2, 2, 3 ),
 ( 0.6250000000000002220, 0.6375000000000000666, 0.6500000000000001332, 0.6624999999999999778, 0.6749999999999999334 ),
 .UNSPECIFIED. ) 
 CURVE ( )  GEOMETRIC_REPRESENTATION_ITEM ( )  RATIONAL_B_SPLINE_CURVE ( ( 0.9999999999999986677, 0.9238795325112880708, 1.000000000000000000, 0.9238795325112867385, 1.000000000000000000, 0.9238795325112867385, 1.000000000000000000, 0.9238795325112874046, 0.9999999999999993339 ) ) 
 REPRESENTATION_ITEM ( '' )  );
#6885 = AXIS2_PLACEMENT_3D ( 'NONE', #9584, #13279, #2144 ) ;
#6886 = ORIENTED_EDGE ( 'NONE', *, *, #15194, .F. ) ;
#6887 = DIRECTION ( 'NONE',  ( 1.000000000000000000, 0.000000000000000000, 0.000000000000000000 ) ) ;
#6888 = AXIS2_PLACEMENT_3D ( 'NONE', #9055, #6538, #13880 ) ;
#6889 = CARTESIAN_POINT ( 'NONE',  ( -4.000000000000000000, -2.309401076758512694, -3.433295621305382461 ) ) ;
#6890 = CARTESIAN_POINT ( 'NONE',  ( 4.458734125000000326, -26.62500000136559564, -1.846868145590734978 ) ) ;
#6891 = DIRECTION ( 'NONE',  ( 0.000000000000000000, 0.000000000000000000, -1.000000000000000000 ) ) ;
#6892 = VECTOR ( 'NONE', #9666, 1000.000000000000000 ) ;
#6893 = CARTESIAN_POINT ( 'NONE',  ( 4.391654775818395251, -2.390265326283149694, -4.125000000000000000 ) ) ;
#6894 = CARTESIAN_POINT ( 'NONE',  ( 6.250000000000002665, -5.051814855409234362, -7.198902722707431145 ) ) ;
#6895 = CARTESIAN_POINT ( 'NONE',  ( 3.033343224707661712, -3.753672977998669946, 1.250000001365594304 ) ) ;
#6896 = ADVANCED_FACE ( 'NONE', ( #10221, #6669 ), #15149, .F. ) ;
#6898 = EDGE_CURVE ( 'NONE', #13770, #10095, #5131, .T. ) ;
#6897 = EDGE_LOOP ( 'NONE', ( #3624, #3189, #4425, #11341, #14973, #13010, #15184, #6160, #11171, #6970, #285, #14481 ) ) ;
#6899 = CLOSED_SHELL ( 'NONE', ( #13377, #1463, #10027, #6781, #6507, #13478, #8268, #12502, #8216, #7329, #2522, #710, #3733, #5561, #13154, #12540, #6599, #2263, #708, #7567, #2470, #4128, #2064, #4293, #6124, #2082, #4802, #8813, #14878, #10945, #15477, #15237, #5942, #9072, #12817, #6402, #8524, #1705, #14965, #10197, #9942, #10926, #15534, #13322, #5467, #9581, #5317, #4048, #5484 ) ) ;
#6900 = ORIENTED_EDGE ( 'NONE', *, *, #5941, .T. ) ;
#6901 = LINE ( 'NONE', #14482, #11844 ) ;
#6902 = ORIENTED_EDGE ( 'NONE', *, *, #5627, .F. ) ;
#6903 = AXIS2_PLACEMENT_3D ( 'NONE', #9752, #7104, #64 ) ;
#6904 = DIRECTION ( 'NONE',  ( 0.000000000000000000, 0.000000000000000000, 1.000000000000000000 ) ) ;
#6905 = PRODUCT_DEFINITION_FORMATION_WITH_SPECIFIED_SOURCE ( 'ANY', '', #8502, .NOT_KNOWN. ) ;
#6906 = CARTESIAN_POINT ( 'NONE',  ( -0.5711823568785977523, -5.381735091635034607, -3.187499997268817609 ) ) ;
#6907 = LINE ( 'NONE', #11728, #1725 ) ;
#6908 = CARTESIAN_POINT ( 'NONE',  ( -5.381735091635034607, 0.5711823568785950878, -8.437499997268814056 ) ) ;
#6909 = PRESENTATION_STYLE_ASSIGNMENT (( #686 ) ) ;
#6910 = VECTOR ( 'NONE', #10576, 1000.000000000000000 ) ;
#6911 = DIRECTION ( 'NONE',  ( 0.000000000000000000, 0.000000000000000000, -1.000000000000000000 ) ) ;
#6912 = CARTESIAN_POINT ( 'NONE',  ( 5.000000000000000888, -24.93750000000000355, -2.071067811865475505 ) ) ;
#6913 = ADVANCED_FACE ( 'NONE', ( #8850 ), #1490, .T. ) ;
#6914 = ORIENTED_EDGE ( 'NONE', *, *, #566, .F. ) ;
#6915 = DIRECTION ( 'NONE',  ( 1.000000000000000000, -0.000000000000000000, 0.000000000000000000 ) ) ;
#6916 = CARTESIAN_POINT ( 'NONE',  ( 2.500000000000000000, 0.000000000000000000, 0.000000000000000000 ) ) ;
#6917 = DIRECTION ( 'NONE',  ( 0.000000000000000000, 0.000000000000000000, -1.000000000000000000 ) ) ;
#6918 = ORIENTED_EDGE ( 'NONE', *, *, #13326, .T. ) ;
#6919 = CARTESIAN_POINT ( 'NONE',  ( 2.071067811865491048, -27.18750000000000000, 4.999999999999985789 ) ) ;
#6920 = EDGE_LOOP ( 'NONE', ( #2378, #8318, #11294, #15860, #10789, #11900 ) ) ;
#6921 = AXIS2_PLACEMENT_3D ( 'NONE', #3187, #1809, #14187 ) ;
#6922 = ORIENTED_EDGE ( 'NONE', *, *, #446, .T. ) ;
#6923 = CARTESIAN_POINT ( 'NONE',  ( 3.753672977998667726, 3.033343224707664820, -0.4999999986344072500 ) ) ;
#6924 = CARTESIAN_POINT ( 'NONE',  ( 3.061616997868383141E-16, -29.87500000273118417, -5.000000000000000000 ) ) ;
#6925 = CARTESIAN_POINT ( 'NONE',  ( -7.500000000000005329, 2.932633423934443151, -0.4709827563909335657 ) ) ;
#6926 = VECTOR ( 'NONE', #14028, 1000.000000000000000 ) ;
#6927 =( REPRESENTATION_RELATIONSHIP ('NONE','NONE', #4176, #790 ) REPRESENTATION_RELATIONSHIP_WITH_TRANSFORMATION ( #7641 )SHAPE_REPRESENTATION_RELATIONSHIP( ) );
#6928 = CARTESIAN_POINT ( 'NONE',  ( -19.99999999999956657, -13.00000000000000178, 8.786575603324269439E-13 ) ) ;
#6929 = DIRECTION ( 'NONE',  ( 0.000000000000000000, 0.000000000000000000, 1.000000000000000000 ) ) ;
#6930 = VECTOR ( 'NONE', #5197, 1000.000000000000227 ) ;
#6931 = DIRECTION ( 'NONE',  ( -0.000000000000000000, -1.000000000000000000, -0.000000000000000000 ) ) ;
#6932 = CARTESIAN_POINT ( 'NONE',  ( 12.67949192431126093, -37.00000000000000711, -61.96152422706632024 ) ) ;
#6933 = EDGE_CURVE ( 'NONE', #9162, #6438, #9744, .T. ) ;
#6934 = CARTESIAN_POINT ( 'NONE',  ( -6.765421556309547668E-13, 40.00000000000000000, 67.49999999999930367 ) ) ;
#6935 = EDGE_CURVE ( 'NONE', #10196, #2292, #4788, .T. ) ;
#6936 = CARTESIAN_POINT ( 'NONE',  ( 1.846868145590735200, -31.50000000136559564, -4.458734124999999437 ) ) ;
#6937 = ADVANCED_FACE ( 'NONE', ( #5205 ), #5912, .F. ) ;
#6938 = EDGE_CURVE ( 'NONE', #5212, #15819, #3980, .T. ) ;
#6939 = CARTESIAN_POINT ( 'NONE',  ( -2.131511515620587272, -3.916244202832140253, -0.6874999986344054737 ) ) ;
#6940 = VERTEX_POINT ( 'NONE', #4470 ) ;
#6941 = UNCERTAINTY_MEASURE_WITH_UNIT (LENGTH_MEASURE( 1.000000000000000082E-05 ), #8215, 'distance_accuracy_value', 'NONE');
#6942 = VECTOR ( 'NONE', #8856, 1000.000000000000000 ) ;
#6943 = LINE ( 'NONE', #13053, #9701 ) ;
#6944 = ORIENTED_EDGE ( 'NONE', *, *, #15306, .F. ) ;
#6945 = ORIENTED_EDGE ( 'NONE', *, *, #5671, .F. ) ;
#6946 = AXIS2_PLACEMENT_3D ( 'NONE', #4949, #1306, #11097 ) ;
#6947 = CARTESIAN_POINT ( 'NONE',  ( 3.152801135295367541, -26.56250000136559564, -3.152801135295367541 ) ) ;
#6948 = CARTESIAN_POINT ( 'NONE',  ( 4.000000000000000000, -2.309401076758516691, -0.4999999999999995559 ) ) ;
#6949 = CIRCLE ( 'NONE', #12809, 2.649999999999992806 ) ;
#6950 = DIRECTION ( 'NONE',  ( -0.000000000000000000, 1.000000000000000000, 0.000000000000000000 ) ) ;
#6951 = FACE_OUTER_BOUND ( 'NONE', #13877, .T. ) ;
#6952 = CARTESIAN_POINT ( 'NONE',  ( 4.276409079477644148, 1.261996585732577891, -6.312499998634407028 ) ) ;
#6953 = CARTESIAN_POINT ( 'NONE',  ( 3.761221015330621587, -3.194220869028280507, 48.77578944492238833 ) ) ;
#6954 = AXIS2_PLACEMENT_3D ( 'NONE', #629, #10483, #12804 ) ;
#6955 = CIRCLE ( 'NONE', #1521, 0.7733184030943203169 ) ;
#6956 = CARTESIAN_POINT ( 'NONE',  ( -3.535533905932738641, -27.37500000000000000, 3.535533905932737309 ) ) ;
#6957 = CARTESIAN_POINT ( 'NONE',  ( 4.391654775818395251, -2.390265326283149694, 0.8749999999999973355 ) ) ;
#6958 = DIRECTION ( 'NONE',  ( -0.000000000000000000, -1.000000000000000000, -0.000000000000000000 ) ) ;
#6959 = CARTESIAN_POINT ( 'NONE',  ( 4.769696007084728073, -13.00000000000000178, 1.500000000000000000 ) ) ;
#6960 = CARTESIAN_POINT ( 'NONE',  ( -3.152801135295367096, -30.06250000136559564, -3.152801135295367541 ) ) ;
#6961 = EDGE_CURVE ( 'NONE', #2882, #10281, #748, .T. ) ;
#6962 = EDGE_LOOP ( 'NONE', ( #14982, #3680, #13608 ) ) ;
#6963 = CARTESIAN_POINT ( 'NONE',  ( -2.100000000000000089, 2.571758278209441957E-16, -0.2800830152838844622 ) ) ;
#6964 = DIRECTION ( 'NONE',  ( -1.000000000000000000, -0.000000000000000000, -0.000000000000000000 ) ) ;
#6965 = VERTEX_POINT ( 'NONE', #835 ) ;
#6966 = ORIENTED_EDGE ( 'NONE', *, *, #2426, .T. ) ;
#6967 = CARTESIAN_POINT ( 'NONE',  ( 7.500000000000004441, -4.330127018922205195, -1.000000000000000888 ) ) ;
#6968 = CARTESIAN_POINT ( 'NONE',  ( -1.846868145590737420, -27.75000000136559564, 4.458734124999999437 ) ) ;
#6969 = DIRECTION ( 'NONE',  ( 0.000000000000000000, 0.000000000000000000, 1.000000000000000000 ) ) ;
#6970 = ORIENTED_EDGE ( 'NONE', *, *, #8773, .F. ) ;
#6972 = AXIS2_PLACEMENT_3D ( 'NONE', #15489, #5936, #848 ) ;
#6971 = CARTESIAN_POINT ( 'NONE',  ( 0.000000000000000000, -13.00000000000000178, 0.000000000000000000 ) ) ;
#6973 = ADVANCED_BREP_SHAPE_REPRESENTATION ( '', ( #3386, #3223 ), #1155 ) ;
#6974 = CARTESIAN_POINT ( 'NONE',  ( 2.730187237215162345E-16, -26.43750000136559564, -4.458734124999999437 ) ) ;
#6975 = CARTESIAN_POINT ( 'NONE',  ( 3.472371940585993855, 2.614027278893175321, -3.320322319201766792 ) ) ;
#6976 = FACE_OUTER_BOUND ( 'NONE', #13252, .T. ) ;
#6977 = CARTESIAN_POINT ( 'NONE',  ( 2.071067811865461294, -30.81249999999999645, -5.000000000000014211 ) ) ;
#6978 = DIRECTION ( 'NONE',  ( 0.000000000000000000, -1.000000000000000000, 0.000000000000000000 ) ) ;
#6979 = EDGE_LOOP ( 'NONE', ( #12956, #11485 ) ) ;
#6980 =( BOUNDED_SURFACE ( )  B_SPLINE_SURFACE ( 3, 2, ( 
 ( #4239, #5383, #3028 ),
 ( #4158, #15249, #12879 ),
 ( #7436, #2939, #12714 ),
 ( #6300, #11214, #6760 ),
 ( #11508, #3782, #9919 ),
 ( #12417, #8729, #11593 ) ),
 .UNSPECIFIED., .F., .F., .F. ) 
 B_SPLINE_SURFACE_WITH_KNOTS ( ( 4, 2, 4 ),
 ( 3, 3 ),
 ( 0.02027752710269158445, 0.02273781595091097299, 0.02519810479913036153 ),
 ( 0.000000000000000000, 1.000000000000000000 ),
 .UNSPECIFIED. ) 
 GEOMETRIC_REPRESENTATION_ITEM ( )  RATIONAL_B_SPLINE_SURFACE ( (
 ( 1.000000000000000000, 0.8047781431712808242, 1.000000000000000000),
 ( 1.000000000000000000, 0.8123773247083928561, 1.000000000000000000),
 ( 1.000000000000000000, 0.8190670192154906326, 1.000000000000000000),
 ( 1.000000000000000000, 0.8192353552912178261, 1.000000000000000000),
 ( 1.000000000000000000, 0.8126132098226825917, 1.000000000000000000),
 ( 1.000000000000000000, 0.8047712465856394770, 1.000000000000000000) ) ) 
 REPRESENTATION_ITEM ( '' )  SURFACE ( )  );
#6981 = SHAPE_REPRESENTATION ( 'Precision Linear Jaw Guides', ( #3223 ), #14881 ) ;
#6982 = EDGE_LOOP ( 'NONE', ( #9556, #9009, #14858, #7856, #3661, #13785 ) ) ;
#6983 = CARTESIAN_POINT ( 'NONE',  ( -115.0000000000000142, -10.00000000000000888, 7.500000000000001776 ) ) ;
#6984 = ORIENTED_EDGE ( 'NONE', *, *, #15393, .T. ) ;
#6985 = DIRECTION ( 'NONE',  ( -1.000000000000000000, 0.000000000000000000, 0.000000000000000000 ) ) ;
#6986 = ADVANCED_FACE ( 'NONE', ( #3340 ), #14670, .T. ) ;
#6987 = EDGE_CURVE ( 'NONE', #11826, #4598, #7986, .T. ) ;
#6988 = DIRECTION ( 'NONE',  ( -1.000000000000000000, -0.000000000000000000, -0.000000000000000000 ) ) ;
#6989 = CARTESIAN_POINT ( 'NONE',  ( 2.131511515620586383, 3.916244202832140253, -0.1874999986344084990 ) ) ;
#6990 = DIRECTION ( 'NONE',  ( 0.000000000000000000, -1.000000000000000000, 0.000000000000000000 ) ) ;
#6991 = CARTESIAN_POINT ( 'NONE',  ( -0.5711823568785978633, -5.381735091635035495, -6.187499997268815832 ) ) ;
#6992 = LINE ( 'NONE', #10553, #5524 ) ;
#6993 = CARTESIAN_POINT ( 'NONE',  ( 3.061616997868383043E-15, 20.00000000000000000, -25.00000000000000000 ) ) ;
#6994 = LINE ( 'NONE', #5530, #4781 ) ;
#6995 = ORIENTED_EDGE ( 'NONE', *, *, #11649, .T. ) ;
#6996 = CARTESIAN_POINT ( 'NONE',  ( -4.336808689942017736E-16, -8.660254037844399733, -9.999999999999998224 ) ) ;
#6997 = CARTESIAN_POINT ( 'NONE',  ( -7.500000000000005329, 4.330127018922194537, -7.422398894150031623 ) ) ;
#6998 = EDGE_LOOP ( 'NONE', ( #1254, #7541, #7678, #4735 ) ) ;
#6999 = CARTESIAN_POINT ( 'NONE',  ( 2.500000000000000000, 2.357898499370433054, -1.951563910473907981E-15 ) ) ;
#7000 = ORIENTED_EDGE ( 'NONE', *, *, #499, .F. ) ;
#7001 = ORIENTED_EDGE ( 'NONE', *, *, #10395, .F. ) ;
#7002 = DIRECTION ( 'NONE',  ( 0.000000000000000000, -0.000000000000000000, 1.000000000000000000 ) ) ;
#7003 = CYLINDRICAL_SURFACE ( 'NONE', #4551, 5.000000000000000888 ) ;
#7004 = DIRECTION ( 'NONE',  ( -0.000000000000000000, 1.000000000000000000, 1.224646799147353207E-16 ) ) ;
#7005 = EDGE_CURVE ( 'NONE', #8373, #5402, #3568, .T. ) ;
#7006 = EDGE_CURVE ( 'NONE', #1214, #13461, #2797, .T. ) ;
#7007 = FACE_OUTER_BOUND ( 'NONE', #1717, .T. ) ;
#7008 = DIRECTION ( 'NONE',  ( 0.000000000000000000, 0.000000000000000000, 1.000000000000000000 ) ) ;
#7009 = CARTESIAN_POINT ( 'NONE',  ( -43.99999999999978684, -9.000000000000001776, -1.500000000000000666 ) ) ;
#7010 = CARTESIAN_POINT ( 'NONE',  ( 10.00000000000098765, -20.00000000000000000, 19.82050807568871065 ) ) ;
#7011 = DIRECTION ( 'NONE',  ( 0.000000000000000000, -1.000000000000000000, 0.000000000000000000 ) ) ;
#7012 = CARTESIAN_POINT ( 'NONE',  ( -6.288404560131955812, -5.029641972278938056, -0.4504974108211986517 ) ) ;
#7013 = CARTESIAN_POINT ( 'NONE',  ( 4.458734124999997661, -28.75000000136559564, 1.846868145590737864 ) ) ;
#7014 = CARTESIAN_POINT ( 'NONE',  ( -4.799145180956616130, 0.5093500532425063732, -0.8749999986344056957 ) ) ;
#7015 = ORIENTED_EDGE ( 'NONE', *, *, #14503, .T. ) ;
#7016 = CARTESIAN_POINT ( 'NONE',  ( 5.335963852943357288, 6.035591050532032042, -7.593821156097325442 ) ) ;
#7017 = EDGE_LOOP ( 'NONE', ( #6335, #5344 ) ) ;
#7018 = EDGE_LOOP ( 'NONE', ( #8770, #6447, #8173, #5770 ) ) ;
#7019 =( NAMED_UNIT ( * ) SI_UNIT ( $, .STERADIAN. ) SOLID_ANGLE_UNIT ( ) );
#7020 = EDGE_LOOP ( 'NONE', ( #14515, #10540, #10302, #4217, #5979, #2639, #4756, #7595, #8104 ) ) ;
#7021 = CARTESIAN_POINT ( 'NONE',  ( -4.458734125000001214, -28.12500000136559564, 1.846868145590734089 ) ) ;
#7022 = CARTESIAN_POINT ( 'NONE',  ( -3.401574460001765221, 4.209348295687701302, -7.687500000000004441 ) ) ;
#7023 = DIRECTION ( 'NONE',  ( 0.000000000000000000, -0.4999999999999993894, 0.8660254037844389297 ) ) ;
#7024 = EDGE_CURVE ( 'NONE', #9050, #7077, #12424, .T. ) ;
#7025 = ADVANCED_FACE ( 'NONE', ( #5757 ), #11653, .F. ) ;
#7026 = CARTESIAN_POINT ( 'NONE',  ( -3.916244202832140253, 2.131511515620587272, -4.937499998634406140 ) ) ;
#7027 = CYLINDRICAL_SURFACE ( 'NONE', #8607, 5.000000000000000888 ) ;
#7028 = AXIS2_PLACEMENT_3D ( 'NONE', #1160, #8540, #10944 ) ;
#7029 = LINE ( 'NONE', #11054, #12606 ) ;
#7030 = CARTESIAN_POINT ( 'NONE',  ( -2.390265326283148806, -4.391654775818394363, 1.624999999999998002 ) ) ;
#7031 = DIRECTION ( 'NONE',  ( -0.000000000000000000, -1.000000000000000000, -0.000000000000000000 ) ) ;
#7032 = CARTESIAN_POINT ( 'NONE',  ( 5.000000000000004441, 5.204748896376250699E-16, -4.250000000000000000 ) ) ;
#7033 = CARTESIAN_POINT ( 'NONE',  ( 4.458734124999999437, -30.43750000136559564, 0.000000000000000000 ) ) ;
#7034 = ORIENTED_EDGE ( 'NONE', *, *, #10134, .T. ) ;
#7035 = CARTESIAN_POINT ( 'NONE',  ( 3.152801135295367541, -23.31250000136559564, -3.152801135295367541 ) ) ;
#7036 = CARTESIAN_POINT ( 'NONE',  ( 0.000000000000000000, 50.00000000000000000, 0.000000000000000000 ) ) ;
#7037 = VERTEX_POINT ( 'NONE', #14180 ) ;
#7038 = VERTEX_POINT ( 'NONE', #3178 ) ;
#7039 = LINE ( 'NONE', #2017, #14433 ) ;
#7040 = CARTESIAN_POINT ( 'NONE',  ( 1.846868145590735200, -30.25000000136559564, -4.458734125000000326 ) ) ;
#7041 = CARTESIAN_POINT ( 'NONE',  ( 0.000000000000000000, 0.000000000000000000, 0.000000000000000000 ) ) ;
#7042 = ORIENTED_EDGE ( 'NONE', *, *, #63, .F. ) ;
#7043 = CARTESIAN_POINT ( 'NONE',  ( 19.99999999999956657, -8.786575603324269439E-13, 0.000000000000000000 ) ) ;
#7044 = EDGE_CURVE ( 'NONE', #8839, #7200, #5647, .T. ) ;
#7045 = DIRECTION ( 'NONE',  ( -1.541976423090495140E-16, 1.000000000000000000, 0.000000000000000000 ) ) ;
#7046 = FACE_OUTER_BOUND ( 'NONE', #10152, .T. ) ;
#7047 = CARTESIAN_POINT ( 'NONE',  ( -4.458734125000000326, -26.25000000136559208, -1.846868145590735644 ) ) ;
#7048 = DIRECTION ( 'NONE',  ( 1.000000000000000000, 1.541976423090495140E-16, -0.000000000000000000 ) ) ;
#7049 = LINE ( 'NONE', #14241, #8500 ) ;
#7050 = CARTESIAN_POINT ( 'NONE',  ( 3.061616997868383141E-16, -30.87500000273118772, -5.000000000000000000 ) ) ;
#7051 = AXIS2_PLACEMENT_3D ( 'NONE', #10835, #11710, #4529 ) ;
#7052 = CARTESIAN_POINT ( 'NONE',  ( 0.000000000000000000, -13.00000000000000178, 0.000000000000000000 ) ) ;
#7053 = VECTOR ( 'NONE', #3197, 1000.000000000000000 ) ;
#7054 = ORIENTED_EDGE ( 'NONE', *, *, #14232, .F. ) ;
#7055 = VERTEX_POINT ( 'NONE', #10694 ) ;
#7056 = CARTESIAN_POINT ( 'NONE',  ( -4.000000000000000000, 0.3987449864459974846, -0.01220643443059782861 ) ) ;
#7057 = ORIENTED_EDGE ( 'NONE', *, *, #14005, .T. ) ;
#7058 = AXIS2_PLACEMENT_3D ( 'NONE', #7906, #12650, #13702 ) ;
#7059 = EDGE_CURVE ( 'NONE', #658, #7410, #8756, .T. ) ;
#7060 = CIRCLE ( 'NONE', #5755, 30.00000000000000711 ) ;
#7061 = LINE ( 'NONE', #14559, #11984 ) ;
#7062 = CARTESIAN_POINT ( 'NONE',  ( 5.000000000000004441, -2.247904837838113790E-16, -2.920263044861759472 ) ) ;
#7063 = ORIENTED_EDGE ( 'NONE', *, *, #13884, .F. ) ;
#7064 = CARTESIAN_POINT ( 'NONE',  ( 4.799145180956616130, -0.5093500532425063732, 0.6250000013655918618 ) ) ;
#7065 = DIRECTION ( 'NONE',  ( 0.000000000000000000, 0.000000000000000000, 1.000000000000000000 ) ) ;
#7066 =( BOUNDED_CURVE ( )  B_SPLINE_CURVE ( 2, ( #1425, #4171, #8798, #7672, #12570, #6528, #1517, #15177, #5309, #6455, #10165 ),
 .UNSPECIFIED., .F., .F. ) 
 B_SPLINE_CURVE_WITH_KNOTS ( ( 3, 2, 2, 2, 2, 3 ),
 ( 0.4545872658012772849, 0.4625000000000000222, 0.4749999999999999778, 0.4874999999999999889, 0.5000000000000000000, 0.5045872658012773293 ),
 .UNSPECIFIED. ) 
 CURVE ( )  GEOMETRIC_REPRESENTATION_ITEM ( )  RATIONAL_B_SPLINE_CURVE ( ( 0.9646335149384808183, 0.9518143178943437865, 1.000000000000000000, 0.9238795325112867385, 1.000000000000000000, 0.9238795325112867385, 1.000000000000000000, 0.9238795325112867385, 1.000000000000000000, 0.9720652146169423968, 0.9646335149384803742 ) ) 
 REPRESENTATION_ITEM ( '' )  );
#7067 = PRODUCT_DEFINITION_SHAPE ( 'NONE', 'NONE',  #6009 ) ;
#7069 = CIRCLE ( 'NONE', #5518, 2.000000000000000888 ) ;
#7068 = CARTESIAN_POINT ( 'NONE',  ( 3.033343224707661712, -3.753672977998669946, 0.2500000013655933606 ) ) ;
#7070 = DIRECTION ( 'NONE',  ( -0.000000000000000000, 1.000000000000000000, 1.224646799147353207E-16 ) ) ;
#7071 = CARTESIAN_POINT ( 'NONE',  ( 2.459698528280935381, -7.240146430416074530, -0.09933465333851865253 ) ) ;
#7072 = EDGE_LOOP ( 'NONE', ( #11633, #7367, #1480, #14513 ) ) ;
#7073 = DIRECTION ( 'NONE',  ( -1.319090325525611458E-16, -1.000000000000000000, 0.000000000000000000 ) ) ;
#7074 = EDGE_CURVE ( 'NONE', #3918, #12974, #11822, .T. ) ;
#7075 = VERTEX_POINT ( 'NONE', #15629 ) ;
#7076 = DIRECTION ( 'NONE',  ( 1.319090325525611458E-16, 1.000000000000000000, -0.000000000000000000 ) ) ;
#7077 = VERTEX_POINT ( 'NONE', #5685 ) ;
#7078 = AXIS2_PLACEMENT_3D ( 'NONE', #7652, #7566, #15153 ) ;
#7079 = ORIENTED_EDGE ( 'NONE', *, *, #14466, .F. ) ;
#7080 = CYLINDRICAL_SURFACE ( 'NONE', #13473, 5.000000000000000000 ) ;
#7081 = DIRECTION ( 'NONE',  ( 0.000000000000000000, 0.000000000000000000, 1.000000000000000000 ) ) ;
#7082 = DIRECTION ( 'NONE',  ( -0.8660254037844383745, 0.5000000000000004441, 0.000000000000000000 ) ) ;
#7083 = CARTESIAN_POINT ( 'NONE',  ( 0.000000000000000000, 37.00000000000000000, 75.00000000000001421 ) ) ;
#7084 =( GEOMETRIC_REPRESENTATION_CONTEXT ( 3 ) GLOBAL_UNCERTAINTY_ASSIGNED_CONTEXT ( ( #6581 ) ) GLOBAL_UNIT_ASSIGNED_CONTEXT ( ( #9620, #13654, #5014 ) ) REPRESENTATION_CONTEXT ( 'NONE', 'WORKASPACE' ) );
#7085 = CARTESIAN_POINT ( 'NONE',  ( 4.391654775818395251, -2.390265326283149694, 2.731183335047404626E-09 ) ) ;
#7086 = CARTESIAN_POINT ( 'NONE',  ( 2.500000000000000000, 1.178949249685213863, -2.042000000000001148 ) ) ;
#7087 = CARTESIAN_POINT ( 'NONE',  ( 0.000000000000000000, -11.00000000000000178, 0.000000000000000000 ) ) ;
#7088 = CARTESIAN_POINT ( 'NONE',  ( 4.458734124999999437, -31.68750000136559564, 0.000000000000000000 ) ) ;
#7089 = AXIS2_PLACEMENT_3D ( 'NONE', #7776, #5493, #6392 ) ;
#7090 = CARTESIAN_POINT ( 'NONE',  ( 3.753672977998667726, 3.033343224707664376, -2.249999998634408804 ) ) ;
#7091 = ORIENTED_EDGE ( 'NONE', *, *, #3407, .F. ) ;
#7092 = LINE ( 'NONE', #11993, #167 ) ;
#7093 = EDGE_CURVE ( 'NONE', #1580, #8519, #8063, .T. ) ;
#7094 = ORIENTED_EDGE ( 'NONE', *, *, #4507, .T. ) ;
#7095 = ORIENTED_EDGE ( 'NONE', *, *, #5433, .T. ) ;
#7096 = EDGE_CURVE ( 'NONE', #10415, #12974, #12064, .T. ) ;
#7097 = SURFACE_STYLE_FILL_AREA ( #15898 ) ;
#7098 = ORIENTED_EDGE ( 'NONE', *, *, #14944, .F. ) ;
#7099 = CARTESIAN_POINT ( 'NONE',  ( 2.730187237215162345E-16, -28.43750000136559564, -4.458734124999999437 ) ) ;
#7100 = CARTESIAN_POINT ( 'NONE',  ( -39.99999999999999289, -9.000000000000001776, 2.500000000001739497 ) ) ;
#7101 = AXIS2_PLACEMENT_3D ( 'NONE', #15790, #10778, #15717 ) ;
#7102 = CARTESIAN_POINT ( 'NONE',  ( 5.200000000000002842, 0.000000000000000000, -2.700000000000000622 ) ) ;
#7103 = AXIS2_PLACEMENT_3D ( 'NONE', #13773, #2871, #7580 ) ;
#7104 = DIRECTION ( 'NONE',  ( -1.000000000000000000, 0.000000000000000000, 0.000000000000000000 ) ) ;
#7105 = FACE_OUTER_BOUND ( 'NONE', #1889, .T. ) ;
#7106 = CARTESIAN_POINT ( 'NONE',  ( -5.000000000000000888, -22.56250000000000000, -2.071067811865475949 ) ) ;
#7107 = CARTESIAN_POINT ( 'NONE',  ( -1.261996585732579224, 4.276409079477648589, -8.062499998634407916 ) ) ;
#7108 = DIRECTION ( 'NONE',  ( -0.000000000000000000, 1.000000000000000000, -0.000000000000000000 ) ) ;
#7109 = CARTESIAN_POINT ( 'NONE',  ( -0.8301538844988668453, -4.780499171557324622, -0.1086890209542362012 ) ) ;
#7110 = CARTESIAN_POINT ( 'NONE',  ( 2.071067811865476394, -22.31250000273118417, 5.000000000000000000 ) ) ;
#7111 = ORIENTED_EDGE ( 'NONE', *, *, #11437, .F. ) ;
#7112 = CIRCLE ( 'NONE', #2431, 3.499999999999999556 ) ;
#7113 = EDGE_CURVE ( 'NONE', #7197, #12835, #9013, .T. ) ;
#7114 = CARTESIAN_POINT ( 'NONE',  ( 2.143131898507869826E-15, 37.00000000000000000, -67.50000000000000000 ) ) ;
#7115 = ORIENTED_EDGE ( 'NONE', *, *, #11371, .F. ) ;
#7116 = ORIENTED_EDGE ( 'NONE', *, *, #2281, .F. ) ;
#7117 = EDGE_CURVE ( 'NONE', #13476, #4620, #2415, .T. ) ;
#7118 = LINE ( 'NONE', #13391, #13640 ) ;
#7119 = CARTESIAN_POINT ( 'NONE',  ( -3.152801135295367985, -29.81250000136559208, 3.152801135295367096 ) ) ;
#7120 = PLANE ( 'NONE',  #6874 ) ;
#7121 = ORIENTED_EDGE ( 'NONE', *, *, #2018, .F. ) ;
#7122 = CARTESIAN_POINT ( 'NONE',  ( 3.061616997868383141E-16, -24.87500000273118417, -4.999999999999999112 ) ) ;
#7123 = CIRCLE ( 'NONE', #155, 2.000000000000000888 ) ;
#7124 = CARTESIAN_POINT ( 'NONE',  ( -0.5974722283283653290, 8.315303285985685022, -0.7026937717022876395 ) ) ;
#7125 = FACE_OUTER_BOUND ( 'NONE', #12315, .T. ) ;
#7126 = DIRECTION ( 'NONE',  ( -0.8191520442889875797, 1.003171929053519570E-16, 0.5735764363510522656 ) ) ;
#7127 = VECTOR ( 'NONE', #15456, 1000.000000000000114 ) ;
#7128 = CARTESIAN_POINT ( 'NONE',  ( 4.458734124999999437, -24.68750000136559564, 0.000000000000000000 ) ) ;
#7129 = AXIS2_PLACEMENT_3D ( 'NONE', #743, #12923, #12999 ) ;
#7130 = CARTESIAN_POINT ( 'NONE',  ( 3.453038570460273071, 2.625189405340834448, -3.535263753543585352 ) ) ;
#7131 = CARTESIAN_POINT ( 'NONE',  ( -6.259644161404860030E-16, -4.618802153517027165, -3.433295621305388234 ) ) ;
#7132 = DIRECTION ( 'NONE',  ( 0.000000000000000000, 1.000000000000000000, 0.000000000000000000 ) ) ;
#7133 = EDGE_CURVE ( 'NONE', #3133, #3171, #5022, .T. ) ;
#7135 = EDGE_CURVE ( 'NONE', #6319, #5667, #6949, .T. ) ;
#7134 = VERTEX_POINT ( 'NONE', #14561 ) ;
#7136 = EDGE_CURVE ( 'NONE', #1523, #13974, #15788, .T. ) ;
#7137 = AXIS2_PLACEMENT_3D ( 'NONE', #12413, #14773, #8566 ) ;
#7138 = ORIENTED_EDGE ( 'NONE', *, *, #586, .T. ) ;
#7139 = CARTESIAN_POINT ( 'NONE',  ( -6.486836893983028318, 4.915077010914117750, -7.231838333420224529 ) ) ;
#7140 = VECTOR ( 'NONE', #9037, 1000.000000000000114 ) ;
#7141 = VERTEX_POINT ( 'NONE', #8442 ) ;
#7142 = CARTESIAN_POINT ( 'NONE',  ( 3.061616997868383141E-16, -26.75000000000000000, -5.000000000000000000 ) ) ;
#7143 = CIRCLE ( 'NONE', #12790, 2.649999999999992806 ) ;
#7144 = LINE ( 'NONE', #6080, #1776 ) ;
#7145 = CARTESIAN_POINT ( 'NONE',  ( 0.5093500532425063732, 4.799145180956616130, -1.124999998634405918 ) ) ;
#7146 = DIRECTION ( 'NONE',  ( 0.000000000000000000, -1.000000000000000000, 0.000000000000000000 ) ) ;
#7147 = CIRCLE ( 'NONE', #14110, 10.00000000000000711 ) ;
#7148 = CARTESIAN_POINT ( 'NONE',  ( -0.5093500532425060401, -4.799145180956616130, 0.1250000013655913900 ) ) ;
#7149 = CARTESIAN_POINT ( 'NONE',  ( 0.000000000000000000, 1.178949249685213863, -2.042000000000001148 ) ) ;
#7150 = CARTESIAN_POINT ( 'NONE',  ( 3.096526599377913413, -6.872473572140724407, -6.360652745248294783E-15 ) ) ;
#7151 = EDGE_LOOP ( 'NONE', ( #9247, #13441 ) ) ;
#7152 = CARTESIAN_POINT ( 'NONE',  ( 0.000000000000000000, 1.178949249685213863, -2.042000000000001148 ) ) ;
#7153 = EDGE_CURVE ( 'NONE', #11683, #12492, #7144, .T. ) ;
#7154 = SURFACE_SIDE_STYLE ('',( #2203 ) ) ;
#7155 = EDGE_LOOP ( 'NONE', ( #4057, #6201, #8222, #6777 ) ) ;
#7156 = FACE_OUTER_BOUND ( 'NONE', #15897, .T. ) ;
#7157 = CIRCLE ( 'NONE', #1718, 2.649999999999992806 ) ;
#7158 = ORIENTED_EDGE ( 'NONE', *, *, #8592, .T. ) ;
#7159 = ORIENTED_EDGE ( 'NONE', *, *, #8812, .F. ) ;
#7160 = CARTESIAN_POINT ( 'NONE',  ( -3.916244202832140253, 2.131511515620587272, -3.187499998634407916 ) ) ;
#7161 = EDGE_LOOP ( 'NONE', ( #11373, #10810, #5922, #813 ) ) ;
#7162 = AXIS2_PLACEMENT_3D ( 'NONE', #10363, #9077, #11325 ) ;
#7163 = CARTESIAN_POINT ( 'NONE',  ( -86.33974596215563224, -97.11324865405184426, 7.500000000000001776 ) ) ;
#7164 = ADVANCED_FACE ( 'NONE', ( #1139 ), #3482, .F. ) ;
#7165 = DIRECTION ( 'NONE',  ( 0.000000000000000000, 0.000000000000000000, 1.000000000000000000 ) ) ;
#7167 = DIRECTION ( 'NONE',  ( -0.000000000000000000, -1.000000000000000000, -0.000000000000000000 ) ) ;
#7166 = VECTOR ( 'NONE', #11676, 1000.000000000000000 ) ;
#7168 = PLANE ( 'NONE',  #511 ) ;
#7169 = CARTESIAN_POINT ( 'NONE',  ( -3.401574460001764777, 4.209348295687701302, 0.4375000027311838346 ) ) ;
#7170 = DIRECTION ( 'NONE',  ( 0.000000000000000000, 0.4999999999999993339, -0.8660254037844390407 ) ) ;
#7171 = FILL_AREA_STYLE_COLOUR ( '', #2024 ) ;
#7172 = CARTESIAN_POINT ( 'NONE',  ( 4.458734124999997661, -30.75000000136559919, 1.846868145590737864 ) ) ;
#7173 = CARTESIAN_POINT ( 'NONE',  ( 3.916244202832140253, -2.131511515620588160, -2.437499998634407028 ) ) ;
#7174 = ORIENTED_EDGE ( 'NONE', *, *, #8975, .T. ) ;
#7175 = CIRCLE ( 'NONE', #13868, 2.649999999999992806 ) ;
#7176 = CARTESIAN_POINT ( 'NONE',  ( 1.282512619719710756, 8.391164935524622948, -7.795653906409119038 ) ) ;
#7177 = VERTEX_POINT ( 'NONE', #14726 ) ;
#7178 = ORIENTED_EDGE ( 'NONE', *, *, #437, .T. ) ;
#7179 =( LENGTH_UNIT ( ) NAMED_UNIT ( * ) SI_UNIT ( .MILLI., .METRE. ) );
#7180 = VERTEX_POINT ( 'NONE', #7298 ) ;
#7181 = CARTESIAN_POINT ( 'NONE',  ( 4.458734124999999437, -25.75000000136559564, 1.846868145590737864 ) ) ;
#7182 = CIRCLE ( 'NONE', #15694, 75.00000000000001421 ) ;
#7183 = CYLINDRICAL_SURFACE ( 'NONE', #6617, 3.499999999999999556 ) ;
#7184 = AXIS2_PLACEMENT_3D ( 'NONE', #3969, #6568, #15225 ) ;
#7185 = FACE_BOUND ( 'NONE', #6555, .T. ) ;
#7186 = CIRCLE ( 'NONE', #12059, 2.100000000000000089 ) ;
#7187 = ADVANCED_FACE ( 'NONE', ( #12368, #2276 ), #1064, .F. ) ;
#7188 = CARTESIAN_POINT ( 'NONE',  ( -4.618802153517020948, -3.000000000000000000, 36.00000000000000711 ) ) ;
#7189 = FACE_BOUND ( 'NONE', #4923, .T. ) ;
#7190 = EDGE_CURVE ( 'NONE', #3174, #9050, #12200, .T. ) ;
#7191 = CARTESIAN_POINT ( 'NONE',  ( 2.500000000000000000, 2.357898499370433054, -1.951563910473907981E-15 ) ) ;
#7192 = CARTESIAN_POINT ( 'NONE',  ( 5.381735091635035495, -0.5711823568785978633, -2.062500000000000888 ) ) ;
#7193 = CARTESIAN_POINT ( 'NONE',  ( -4.999999999999844569, 1.272547481429019856, -3.586597482644647616 ) ) ;
#7194 = CARTESIAN_POINT ( 'NONE',  ( 4.104504678892250347, -2.845098865571579871, -0.009045026986704146621 ) ) ;
#7195 = CARTESIAN_POINT ( 'NONE',  ( 3.152801135295366208, -30.56250000136559564, 3.152801135295367985 ) ) ;
#7196 = CARTESIAN_POINT ( 'NONE',  ( 1.261996585732578113, -4.276409079477644148, 1.187500001365592750 ) ) ;
#7197 = VERTEX_POINT ( 'NONE', #10923 ) ;
#7198 = CARTESIAN_POINT ( 'NONE',  ( -114.9999999999999858, -109.4337567297407219, 17.50000000000000000 ) ) ;
#7199 = ORIENTED_EDGE ( 'NONE', *, *, #119, .F. ) ;
#7200 = VERTEX_POINT ( 'NONE', #28 ) ;
#7201 = DIRECTION ( 'NONE',  ( 0.000000000000000000, 0.000000000000000000, 1.000000000000000000 ) ) ;
#7202 = AXIS2_PLACEMENT_3D ( 'NONE', #6008, #10934, #15872 ) ;
#7203 = CARTESIAN_POINT ( 'NONE',  ( -1.846868145590734756, -29.12500000136559919, -4.458734125000000326 ) ) ;
#7204 = CYLINDRICAL_SURFACE ( 'NONE', #8172, 1.999999999999998668 ) ;
#7205 = VERTEX_POINT ( 'NONE', #9871 ) ;
#7206 = CYLINDRICAL_SURFACE ( 'NONE', #6347, 10.00000000000000711 ) ;
#7207 = VECTOR ( 'NONE', #257, 1000.000000000000000 ) ;
#7208 = CARTESIAN_POINT ( 'NONE',  ( -44.99999999999999289, -11.00000000000000178, -3.999999999999170885 ) ) ;
#7209 = FACE_BOUND ( 'NONE', #5935, .T. ) ;
#7210 = LINE ( 'NONE', #2485, #15825 ) ;
#7211 = EDGE_CURVE ( 'NONE', #2517, #2401, #13985, .T. ) ;
#7212 = CARTESIAN_POINT ( 'NONE',  ( 3.152801135295367541, -22.56250000136559564, -3.152801135295367541 ) ) ;
#7213 = AXIS2_PLACEMENT_3D ( 'NONE', #4958, #8689, #1319 ) ;
#7214 = CARTESIAN_POINT ( 'NONE',  ( -9.184850993605147944E-16, -28.37500000273118772, 5.000000000000000000 ) ) ;
#7215 = PLANE ( 'NONE',  #3845 ) ;
#7216 = CARTESIAN_POINT ( 'NONE',  ( 3.401574460001763445, -4.209348295687703079, -6.062499997268814056 ) ) ;
#7217 = FACE_BOUND ( 'NONE', #12920, .T. ) ;
#7218 = VECTOR ( 'NONE', #15280, 1000.000000000000000 ) ;
#7219 = VERTEX_POINT ( 'NONE', #12681 ) ;
#7220 = AXIS2_PLACEMENT_3D ( 'NONE', #9266, #11137, #14192 ) ;
#7221 = ORIENTED_EDGE ( 'NONE', *, *, #9727, .F. ) ;
#7222 = CYLINDRICAL_SURFACE ( 'NONE', #414, 5.999999999999991118 ) ;
#7223 = VERTEX_POINT ( 'NONE', #191 ) ;
#7224 = CARTESIAN_POINT ( 'NONE',  ( -67.50000000000000000, 37.00000000000000000, 2.649999999999285816 ) ) ;
#7225 = EDGE_CURVE ( 'NONE', #3269, #3229, #4046, .T. ) ;
#7226 = EDGE_CURVE ( 'NONE', #3694, #1275, #6168, .T. ) ;
#7227 = EDGE_CURVE ( 'NONE', #2247, #9162, #9079, .T. ) ;
#7228 = CARTESIAN_POINT ( 'NONE',  ( 39.69153896976634144, -4.098233149437865208, 28.32796736983516794 ) ) ;
#7229 = AXIS2_PLACEMENT_3D ( 'NONE', #11255, #11100, #7473 ) ;
#7230 = CARTESIAN_POINT ( 'NONE',  ( 1.261996585732578113, -4.276409079477644148, -1.562499998634406140 ) ) ;
#7231 = CARTESIAN_POINT ( 'NONE',  ( -21.01110699893041911, -7.999999999999996447, -36.39230484541334221 ) ) ;
#7232 = CARTESIAN_POINT ( 'NONE',  ( -3.916244202832140253, 2.131511515620587272, -2.187499998634407028 ) ) ;
#7233 = SURFACE_STYLE_USAGE ( .BOTH. , #12207 ) ;
#7234 = ORIENTED_EDGE ( 'NONE', *, *, #5993, .T. ) ;
#7235 = DIRECTION ( 'NONE',  ( -6.938893903907228378E-16, -1.000000000000000000, -0.000000000000000000 ) ) ;
#7236 =( REPRESENTATION_RELATIONSHIP ('NONE','NONE', #4176, #790 ) REPRESENTATION_RELATIONSHIP_WITH_TRANSFORMATION ( #12536 )SHAPE_REPRESENTATION_RELATIONSHIP( ) );
#7237 = PRESENTATION_STYLE_ASSIGNMENT (( #13346 ) ) ;
#7238 = VERTEX_POINT ( 'NONE', #516 ) ;
#7239 = CARTESIAN_POINT ( 'NONE',  ( -2.390265326283148806, -4.391654775818394363, -1.375000000000001332 ) ) ;
#7240 = DIRECTION ( 'NONE',  ( 0.000000000000000000, 0.000000000000000000, -1.000000000000000000 ) ) ;
#7241 = ORIENTED_EDGE ( 'NONE', *, *, #892, .T. ) ;
#7242 = CARTESIAN_POINT ( 'NONE',  ( -3.916244202832140253, 2.131511515620587272, -4.187499998634405252 ) ) ;
#7243 = ADVANCED_FACE ( 'NONE', ( #5436, #2670 ), #352, .F. ) ;
#7244 = DIRECTION ( 'NONE',  ( 0.000000000000000000, 0.000000000000000000, -1.000000000000000000 ) ) ;
#7245 = DIRECTION ( 'NONE',  ( 0.8660254037844387076, -0.000000000000000000, -0.4999999999999998890 ) ) ;
#7246 = CARTESIAN_POINT ( 'NONE',  ( 0.000000000000000000, 0.000000000000000000, 4.000000000000000000 ) ) ;
#7247 = DIRECTION ( 'NONE',  ( 0.4999999999999997224, 1.734723475976807094E-15, 0.8660254037844387076 ) ) ;
#7248 = CARTESIAN_POINT ( 'NONE',  ( -1.415196051561583790, 4.795541693661363958, -0.6249999972688171646 ) ) ;
#7249 = FACE_OUTER_BOUND ( 'NONE', #12934, .T. ) ;
#7250 = CARTESIAN_POINT ( 'NONE',  ( -9.184850993605147944E-16, -22.37500000273118417, 5.000000000000000000 ) ) ;
#7251 = CARTESIAN_POINT ( 'NONE',  ( 2.730187237215162345E-16, -26.43750000136559564, -4.458734124999999437 ) ) ;
#7252 = CARTESIAN_POINT ( 'NONE',  ( 2.131511515620586383, 3.916244202832140253, -3.187499998634407916 ) ) ;
#7253 = DIRECTION ( 'NONE',  ( 0.000000000000000000, 1.000000000000000000, 0.000000000000000000 ) ) ;
#7254 = ORIENTED_EDGE ( 'NONE', *, *, #2569, .T. ) ;
#7255 = EDGE_LOOP ( 'NONE', ( #15509, #2416 ) ) ;
#7256 =( NAMED_UNIT ( * ) SI_UNIT ( $, .STERADIAN. ) SOLID_ANGLE_UNIT ( ) );
#7257 = ORIENTED_EDGE ( 'NONE', *, *, #5223, .F. ) ;
#7258 = CARTESIAN_POINT ( 'NONE',  ( -3.152801135295367096, -24.31250000136559564, -3.152801135295367541 ) ) ;
#7259 = CARTESIAN_POINT ( 'NONE',  ( 6.123233995736766282E-16, -32.00000000000000000, -5.000000000000000000 ) ) ;
#7260 = CARTESIAN_POINT ( 'NONE',  ( 0.000000000000000000, 37.00000000000000000, 0.000000000000000000 ) ) ;
#7261 = DIRECTION ( 'NONE',  ( 0.000000000000000000, 1.000000000000000000, 0.000000000000000000 ) ) ;
#7262 = CARTESIAN_POINT ( 'NONE',  ( 2.143131898507869826E-15, 37.00000000000000000, -70.14999999999999147 ) ) ;
#7263 = LINE ( 'NONE', #1182, #1244 ) ;
#7264 = CARTESIAN_POINT ( 'NONE',  ( -3.401574460001764777, 4.209348295687701302, -2.687500000000003553 ) ) ;
#7265 = CARTESIAN_POINT ( 'NONE',  ( 0.000000000000000000, 0.000000000000000000, -0.3080913168122742518 ) ) ;
#7266 = CARTESIAN_POINT ( 'NONE',  ( -2.975210800253060839, -3.755114819930441161, -0.1516074998685549846 ) ) ;
#7267 = CARTESIAN_POINT ( 'NONE',  ( -4.458734125000000326, -28.00000000136559564, -1.846868145590735644 ) ) ;
#7268 = CARTESIAN_POINT ( 'NONE',  ( -3.916244202832140253, 2.131511515620587272, -1.187499998634405918 ) ) ;
#7269 = ORIENTED_EDGE ( 'NONE', *, *, #3853, .T. ) ;
#7270 = LINE ( 'NONE', #12171, #6075 ) ;
#7271 = ORIENTED_EDGE ( 'NONE', *, *, #13132, .T. ) ;
#7272 = VERTEX_POINT ( 'NONE', #8833 ) ;
#7273 = CARTESIAN_POINT ( 'NONE',  ( -99.99999999999998579, -25.00000000000000711, -17.50000000000000000 ) ) ;
#7274 = CARTESIAN_POINT ( 'NONE',  ( -1.846868145590734756, -24.12500000136559919, -4.458734125000000326 ) ) ;
#7275 = EDGE_CURVE ( 'NONE', #2433, #11572, #2756, .T. ) ;
#7276 = DIRECTION ( 'NONE',  ( -0.8660254037844381525, 0.000000000000000000, -0.5000000000000007772 ) ) ;
#7277 = ORIENTED_EDGE ( 'NONE', *, *, #4313, .T. ) ;
#7278 = CARTESIAN_POINT ( 'NONE',  ( 4.896370289181515290, -5.000000000000000000, 48.48076211353313170 ) ) ;
#7279 = LINE ( 'NONE', #12027, #1255 ) ;
#7280 = DIRECTION ( 'NONE',  ( -1.000000000000000000, 0.000000000000000000, 0.000000000000000000 ) ) ;
#7281 = DIRECTION ( 'NONE',  ( 0.000000000000000000, 1.000000000000000000, -1.471414886128461471E-15 ) ) ;
#7282 = CARTESIAN_POINT ( 'NONE',  ( 4.458734125000000326, -22.62500000136559564, -1.846868145590734978 ) ) ;
#7283 = PLANE ( 'NONE',  #3461 ) ;
#7284 = FACE_OUTER_BOUND ( 'NONE', #2494, .T. ) ;
#7285 = CARTESIAN_POINT ( 'NONE',  ( 3.535533905932738197, -30.87500000000000000, -3.535533905932738197 ) ) ;
#7286 = DIRECTION ( 'NONE',  ( 1.000000000000000000, 0.000000000000000000, 0.000000000000000000 ) ) ;
#7287 = LINE ( 'NONE', #15702, #11039 ) ;
#7288 = CARTESIAN_POINT ( 'NONE',  ( 0.2500000000000002220, 0.000000000000000000, 0.000000000000000000 ) ) ;
#7289 = VERTEX_POINT ( 'NONE', #6411 ) ;
#7290 =( NAMED_UNIT ( * ) SI_UNIT ( $, .STERADIAN. ) SOLID_ANGLE_UNIT ( ) );
#7292 = ORIENTED_EDGE ( 'NONE', *, *, #13177, .F. ) ;
#7291 = ADVANCED_FACE ( 'NONE', ( #3889 ), #2941, .T. ) ;
#7293 = DIRECTION ( 'NONE',  ( 0.000000000000000000, 0.000000000000000000, -1.000000000000000000 ) ) ;
#7294 = EDGE_CURVE ( 'NONE', #4992, #1523, #7263, .T. ) ;
#7295 = EDGE_LOOP ( 'NONE', ( #10431, #4466, #3005, #10115 ) ) ;
#7296 = CARTESIAN_POINT ( 'NONE',  ( -1.154700538379218600, -35.00000000000000000, -34.00000000000000000 ) ) ;
#7297 = DIRECTION ( 'NONE',  ( 0.000000000000000000, 0.000000000000000000, -1.000000000000000000 ) ) ;
#7298 = CARTESIAN_POINT ( 'NONE',  ( -91.33974596215558961, -105.7735026918962404, -17.50000000000000000 ) ) ;
#7299 = AXIS2_PLACEMENT_3D ( 'NONE', #10108, #12832, #15282 ) ;
#7300 = CARTESIAN_POINT ( 'NONE',  ( 2.071067811865468844, -27.81250000000000000, -5.000000000000007994 ) ) ;
#7301 = CARTESIAN_POINT ( 'NONE',  ( 0.000000000000000000, -20.00000000000000000, 0.000000000000000000 ) ) ;
#7302 = CARTESIAN_POINT ( 'NONE',  ( 1.261996585732578113, -4.276409079477644148, 0.1875000013655918341 ) ) ;
#7303 = DIRECTION ( 'NONE',  ( 0.000000000000000000, 0.000000000000000000, 1.000000000000000000 ) ) ;
#7304 = CARTESIAN_POINT ( 'NONE',  ( 1.211595439868045521, -7.960739084487663320, -0.4504974108212069228 ) ) ;
#7305 = DIRECTION ( 'NONE',  ( 0.000000000000000000, 0.000000000000000000, 1.000000000000000000 ) ) ;
#7306 = FILL_AREA_STYLE_COLOUR ( '', #10238 ) ;
#7307 = EDGE_CURVE ( 'NONE', #13461, #1214, #10305, .T. ) ;
#7308 = ORIENTED_EDGE ( 'NONE', *, *, #3902, .F. ) ;
#7309 = CARTESIAN_POINT ( 'NONE',  ( -4.209348295687703079, -3.401574460001763445, -1.437500000000002220 ) ) ;
#7310 = VERTEX_POINT ( 'NONE', #2084 ) ;
#7311 = EDGE_CURVE ( 'NONE', #5426, #5955, #15828, .T. ) ;
#7312 = EDGE_LOOP ( 'NONE', ( #11973, #198, #6686, #10407 ) ) ;
#7313 = CARTESIAN_POINT ( 'NONE',  ( 4.276409079477644148, 1.261996585732577891, -3.562499998634407916 ) ) ;
#7314 = CARTESIAN_POINT ( 'NONE',  ( 0.000000000000000000, 0.000000000000000000, -25.03750572909317285 ) ) ;
#7315 = DIRECTION ( 'NONE',  ( -0.4999999999999998335, 0.000000000000000000, -0.8660254037844387076 ) ) ;
#7316 = DIRECTION ( 'NONE',  ( 0.000000000000000000, 0.000000000000000000, -1.000000000000000000 ) ) ;
#7317 = DIRECTION ( 'NONE',  ( -0.000000000000000000, 1.000000000000000000, -0.000000000000000000 ) ) ;
#7318 = CARTESIAN_POINT ( 'NONE',  ( -2.100000000000000089, 2.571758278209441957E-16, -4.694516984716113228 ) ) ;
#7319 =( NAMED_UNIT ( * ) PLANE_ANGLE_UNIT ( ) SI_UNIT ( $, .RADIAN. ) );
#7320 = APPLICATION_CONTEXT ( 'automotive_design' ) ;
#7321 = FACE_OUTER_BOUND ( 'NONE', #9289, .T. ) ;
#7322 = CARTESIAN_POINT ( 'NONE',  ( -8.190561711645485556E-16, -24.93750000136559564, 4.458734124999999437 ) ) ;
#7323 = CARTESIAN_POINT ( 'NONE',  ( 2.730187237215162345E-16, -23.18750000136559564, -4.458734124999999437 ) ) ;
#7324 = CARTESIAN_POINT ( 'NONE',  ( -1.261996585732579224, 4.276409079477648589, -6.062499998634407028 ) ) ;
#7325 = DIRECTION ( 'NONE',  ( -0.000000000000000000, 1.000000000000000000, -0.000000000000000000 ) ) ;
#7326 = EDGE_CURVE ( 'NONE', #946, #7457, #4830, .T. ) ;
#7327 = ORIENTED_EDGE ( 'NONE', *, *, #12032, .T. ) ;
#7328 = ORIENTED_EDGE ( 'NONE', *, *, #11336, .T. ) ;
#7329 = ADVANCED_FACE ( 'NONE', ( #10818 ), #9754, .F. ) ;
#7330 = DIRECTION ( 'NONE',  ( 1.000000000000000000, 0.000000000000000000, 0.000000000000000000 ) ) ;
#7331 = ORIENTED_EDGE ( 'NONE', *, *, #10252, .F. ) ;
#7332 = DIRECTION ( 'NONE',  ( -8.881784197001252323E-15, 0.000000000000000000, 1.000000000000000000 ) ) ;
#7333 = DIRECTION ( 'NONE',  ( 0.000000000000000000, 1.000000000000000000, 0.000000000000000000 ) ) ;
#7334 = MECHANICAL_DESIGN_GEOMETRIC_PRESENTATION_REPRESENTATION (  '', ( #14306 ), #13498 ) ;
#7335 = CARTESIAN_POINT ( 'NONE',  ( 0.000000000000000000, 0.000000000000000000, 0.000000000000000000 ) ) ;
#7336 = DIRECTION ( 'NONE',  ( 0.000000000000000000, 0.000000000000000000, 1.000000000000000000 ) ) ;
#7337 = CARTESIAN_POINT ( 'NONE',  ( -3.535533905932737309, -23.62500000000000000, -3.535533905932738197 ) ) ;
#7338 = CARTESIAN_POINT ( 'NONE',  ( 2.390265326283148806, 4.391654775818395251, -1.875000000000001776 ) ) ;
#7339 = DIRECTION ( 'NONE',  ( 0.000000000000000000, -1.000000000000000000, 0.000000000000000000 ) ) ;
#7340 = CARTESIAN_POINT ( 'NONE',  ( -1.599579652451927014, -4.558710419355938015, -0.1233474730213283688 ) ) ;
#7341 = CARTESIAN_POINT ( 'NONE',  ( 2.730187237215162345E-16, -28.18750000136559564, -4.458734124999999437 ) ) ;
#7342 = CARTESIAN_POINT ( 'NONE',  ( 2.131511515620586383, 3.916244202832140253, -1.437499998634406140 ) ) ;
#7343 = ORIENTED_EDGE ( 'NONE', *, *, #3088, .F. ) ;
#7344 = DIRECTION ( 'NONE',  ( 0.8660254037844374864, -0.5000000000000018874, 0.000000000000000000 ) ) ;
#7345 = ORIENTED_EDGE ( 'NONE', *, *, #1206, .F. ) ;
#7346 = ORIENTED_EDGE ( 'NONE', *, *, #8695, .T. ) ;
#7347 = CARTESIAN_POINT ( 'NONE',  ( -21.01110699893041556, -1.230770033143087371E-15, -33.74230484541335073 ) ) ;
#7348 = EDGE_CURVE ( 'NONE', #2510, #7839, #7029, .T. ) ;
#7349 = AXIS2_PLACEMENT_3D ( 'NONE', #58, #4973, #8707 ) ;
#7350 = CARTESIAN_POINT ( 'NONE',  ( 3.152801135295366208, -25.56250000136559564, 3.152801135295367985 ) ) ;
#7351 = CARTESIAN_POINT ( 'NONE',  ( -5.725490332117410652, 0.000000000000000000, 9.916840153471811803 ) ) ;
#7352 = STYLED_ITEM ( 'NONE', ( #4566 ), #13909 ) ;
#7353 = EDGE_LOOP ( 'NONE', ( #7138, #7895, #1148, #564 ) ) ;
#7354 = LINE ( 'NONE', #10985, #10480 ) ;
#7355 = DIRECTION ( 'NONE',  ( -0.000000000000000000, -1.000000000000000000, -0.000000000000000000 ) ) ;
#7356 = CARTESIAN_POINT ( 'NONE',  ( 19.99999999999956657, -8.786575603324269439E-13, 1.500000000000000000 ) ) ;
#7357 = FACE_BOUND ( 'NONE', #6114, .T. ) ;
#7358 = CARTESIAN_POINT ( 'NONE',  ( -3.152801135295367985, -23.06250000136559564, 3.152801135295367096 ) ) ;
#7359 = VECTOR ( 'NONE', #14257, 1000.000000000000000 ) ;
#7360 = DIRECTION ( 'NONE',  ( 0.000000000000000000, 1.000000000000000000, -0.000000000000000000 ) ) ;
#7361 = EDGE_CURVE ( 'NONE', #15747, #946, #8507, .T. ) ;
#7362 = CARTESIAN_POINT ( 'NONE',  ( 5.000000000000000000, -30.12500000273118417, 0.000000000000000000 ) ) ;
#7363 = VECTOR ( 'NONE', #9642, 1000.000000000000114 ) ;
#7364 = CARTESIAN_POINT ( 'NONE',  ( -28.86751345948126257, -37.00000000000000711, -50.00000000000000711 ) ) ;
#7365 = FACE_OUTER_BOUND ( 'NONE', #10918, .T. ) ;
#7366 = LINE ( 'NONE', #14795, #5819 ) ;
#7367 = ORIENTED_EDGE ( 'NONE', *, *, #2620, .T. ) ;
#7368 = ORIENTED_EDGE ( 'NONE', *, *, #5447, .F. ) ;
#7369 = CARTESIAN_POINT ( 'NONE',  ( -1.317756351988340180, 3.857995168970202116, -0.04852650426601388955 ) ) ;
#7370 = VECTOR ( 'NONE', #9454, 1000.000000000000000 ) ;
#7371 = VERTEX_POINT ( 'NONE', #14530 ) ;
#7372 = CARTESIAN_POINT ( 'NONE',  ( 3.678949249685231848, 5.299604027854762026E-17, 0.000000000000000000 ) ) ;
#7373 = AXIS2_PLACEMENT_3D ( 'NONE', #8829, #11395, #4205 ) ;
#7374 = DIRECTION ( 'NONE',  ( -0.000000000000000000, 1.000000000000000000, 0.000000000000000000 ) ) ;
#7375 = ADVANCED_FACE ( 'NONE', ( #15675 ), #4589, .F. ) ;
#7376 = CARTESIAN_POINT ( 'NONE',  ( -1.261996585732579224, 4.276409079477648589, -2.062499998634406584 ) ) ;
#7377 = EDGE_CURVE ( 'NONE', #11041, #7205, #3582, .T. ) ;
#7378 = CIRCLE ( 'NONE', #13293, 2.000000000000000888 ) ;
#7379 = CARTESIAN_POINT ( 'NONE',  ( 3.916244202832140253, -2.131511515620588160, -2.687499998634407028 ) ) ;
#7380 = CARTESIAN_POINT ( 'NONE',  ( 2.500000000000000000, -2.629050547790028551E-15, -2.041999999999999815 ) ) ;
#7381 = CARTESIAN_POINT ( 'NONE',  ( 10.00000000000098765, -13.00000000000000178, 19.82050807568871065 ) ) ;
#7382 = CIRCLE ( 'NONE', #6602, 2.499999999999998668 ) ;
#7383 = DIRECTION ( 'NONE',  ( 0.000000000000000000, 0.000000000000000000, 1.000000000000000000 ) ) ;
#7384 = CONICAL_SURFACE ( 'NONE', #15863, 4.174999999999999822, 0.9599310885968795892 ) ;
#7385 = DIRECTION ( 'NONE',  ( 0.000000000000000000, 0.000000000000000000, 1.000000000000000000 ) ) ;
#7386 = VERTEX_POINT ( 'NONE', #1265 ) ;
#7387 = CARTESIAN_POINT ( 'NONE',  ( 4.211405965630455661, 2.460463115436283932, -3.751298928144577882 ) ) ;
#7388 = DIRECTION ( 'NONE',  ( 0.000000000000000000, 1.000000000000000000, 0.000000000000000000 ) ) ;
#7389 = EDGE_LOOP ( 'NONE', ( #11802, #3051 ) ) ;
#7390 = CARTESIAN_POINT ( 'NONE',  ( 3.753672977998667726, 3.033343224707664820, -4.499999998634407028 ) ) ;
#7391 =( BOUNDED_CURVE ( )  B_SPLINE_CURVE ( 2, ( #14746, #15066, #13506, #8616, #10142, #2444, #8778, #9890, #1400 ),
 .UNSPECIFIED., .F., .F. ) 
 B_SPLINE_CURVE_WITH_KNOTS ( ( 3, 2, 2, 2, 3 ),
 ( 0.02500000000000002220, 0.03750000000000003331, 0.05000000000000004441, 0.06250000000000005551, 0.07500000000000006661 ),
 .UNSPECIFIED. ) 
 CURVE ( )  GEOMETRIC_REPRESENTATION_ITEM ( )  RATIONAL_B_SPLINE_CURVE ( ( 0.9999999999999998890, 0.9238795325112868495, 1.000000000000000000, 0.9238795325112867385, 1.000000000000000000, 0.9238795325112867385, 1.000000000000000000, 0.9238795325112862944, 1.000000000000000444 ) ) 
 REPRESENTATION_ITEM ( '' )  );
#7392 = AXIS2_PLACEMENT_3D ( 'NONE', #11591, #3992, #8944 ) ;
#7393 = DIRECTION ( 'NONE',  ( -0.000000000000000000, -0.000000000000000000, -1.000000000000000000 ) ) ;
#7394 = PRODUCT_DEFINITION_SHAPE ( 'NONE', 'NONE',  #15987 ) ;
#7395 = AXIS2_PLACEMENT_3D ( 'NONE', #401, #5169, #14953 ) ;
#7396 = CARTESIAN_POINT ( 'NONE',  ( -3.033343224707664820, 3.753672977998667726, -7.999999998634411469 ) ) ;
#7397 = DIRECTION ( 'NONE',  ( 0.000000000000000000, 1.000000000000000000, 0.000000000000000000 ) ) ;
#7398 = CARTESIAN_POINT ( 'NONE',  ( -21.01110699893060030, 0.000000000000000000, 36.39230484541324273 ) ) ;
#7399 = EDGE_CURVE ( 'NONE', #8451, #2220, #8796, .T. ) ;
#7400 = UNCERTAINTY_MEASURE_WITH_UNIT (LENGTH_MEASURE( 1.000000000000000082E-05 ), #14406, 'distance_accuracy_value', 'NONE');
#7401 = CARTESIAN_POINT ( 'NONE',  ( 0.000000000000000000, 0.000000000000000000, 0.000000000000000000 ) ) ;
#7402 = CARTESIAN_POINT ( 'NONE',  ( -2.390265326283148806, -4.391654775818394363, 0.7500000027311839457 ) ) ;
#7403 = DIRECTION ( 'NONE',  ( -0.4999999999999997224, 8.673617379884035472E-16, -0.8660254037844387076 ) ) ;
#7404 = AXIS2_PLACEMENT_3D ( 'NONE', #8478, #14689, #12087 ) ;
#7405 = CARTESIAN_POINT ( 'NONE',  ( -4.458734124999999437, -27.25000000136559564, -1.846868145590735644 ) ) ;
#7406 = CARTESIAN_POINT ( 'NONE',  ( 3.152801135295367541, -24.31250000136559564, -3.152801135295367541 ) ) ;
#7407 = CARTESIAN_POINT ( 'NONE',  ( -2.131511515620587272, -3.916244202832140253, -3.687499998634407916 ) ) ;
#7408 = CARTESIAN_POINT ( 'NONE',  ( 0.000000000000000000, 0.000000000000000000, 0.000000000000000000 ) ) ;
#7409 = ORIENTED_EDGE ( 'NONE', *, *, #15324, .F. ) ;
#7410 = VERTEX_POINT ( 'NONE', #238 ) ;
#7411 = AXIS2_PLACEMENT_3D ( 'NONE', #7208, #5907, #1203 ) ;
#7412 = AXIS2_PLACEMENT_3D ( 'NONE', #12884, #698, #5624 ) ;
#7413 = CARTESIAN_POINT ( 'NONE',  ( 0.000000000000000000, 0.000000000000000000, 0.000000000000000000 ) ) ;
#7414 = VERTEX_POINT ( 'NONE', #13867 ) ;
#7415 = CARTESIAN_POINT ( 'NONE',  ( 3.152801135295366208, -23.81250000136559564, 3.152801135295367985 ) ) ;
#7416 = CYLINDRICAL_SURFACE ( 'NONE', #3259, 5.000000000000000000 ) ;
#7417 = CARTESIAN_POINT ( 'NONE',  ( 5.000000000000000888, -30.06250000273118417, -2.071067811865475505 ) ) ;
#7418 = CIRCLE ( 'NONE', #452, 2.649999999999992806 ) ;
#7419 = EDGE_CURVE ( 'NONE', #10129, #14753, #5226, .T. ) ;
#7420 = CARTESIAN_POINT ( 'NONE',  ( -36.99999999999999289, -13.00000000000000178, -3.999999999999170885 ) ) ;
#7421 = CARTESIAN_POINT ( 'NONE',  ( 2.500000000000000000, 1.178949249685218525, 2.041999999999999371 ) ) ;
#7422 = ADVANCED_FACE ( 'NONE', ( #14937 ), #3769, .T. ) ;
#7423 = ADVANCED_FACE ( 'NONE', ( #1515 ), #8957, .F. ) ;
#7424 = CARTESIAN_POINT ( 'NONE',  ( 47.32050807568879947, -37.00000000000000711, -41.96152422706630603 ) ) ;
#7425 = CARTESIAN_POINT ( 'NONE',  ( 4.209348295687701302, 3.401574460001765665, -0.9375000000000018874 ) ) ;
#7426 = DIRECTION ( 'NONE',  ( 0.000000000000000000, -0.5000000000000012212, -0.8660254037844380415 ) ) ;
#7427 = CARTESIAN_POINT ( 'NONE',  ( -4.009547343616874926, -2.543570988302763514, -0.1814977198071575648 ) ) ;
#7428 = CARTESIAN_POINT ( 'NONE',  ( -1.846868145590737420, -26.75000000136559564, 4.458734124999999437 ) ) ;
#7429 = B_SPLINE_CURVE_WITH_KNOTS ( 'NONE', 3,
 ( #411, #11544, #337, #5250, #3071, #5176 ),
 .UNSPECIFIED., .F., .F.,
 ( 4, 2, 4 ),
 ( 0.002365888236228001588, 0.003551327329835089319, 0.004736766423442177049 ),
 .UNSPECIFIED. ) ;
#7430 = CARTESIAN_POINT ( 'NONE',  ( 3.916244202832140253, -2.131511515620588160, -3.687499998634407916 ) ) ;
#7431 = ORIENTED_EDGE ( 'NONE', *, *, #4296, .F. ) ;
#7432 = CARTESIAN_POINT ( 'NONE',  ( 16.49999999999956657, -8.786575603324269439E-13, 1.500000000000000000 ) ) ;
#7433 = ORIENTED_EDGE ( 'NONE', *, *, #762, .T. ) ;
#7434 = VECTOR ( 'NONE', #12943, 1000.000000000000000 ) ;
#7435 = ORIENTED_EDGE ( 'NONE', *, *, #9886, .T. ) ;
#7436 = CARTESIAN_POINT ( 'NONE',  ( -4.000000000000000000, 0.8730739991738342143, -3.223134629628428893 ) ) ;
#7437 = CARTESIAN_POINT ( 'NONE',  ( -3.152801135295367985, -22.81250000136559564, 3.152801135295367096 ) ) ;
#7438 = CARTESIAN_POINT ( 'NONE',  ( 6.123233995736766282E-16, -20.00000000000000000, -5.000000000000000000 ) ) ;
#7439 = ORIENTED_EDGE ( 'NONE', *, *, #15652, .T. ) ;
#7440 = AXIS2_PLACEMENT_3D ( 'NONE', #12633, #9100, #1576 ) ;
#7441 = CARTESIAN_POINT ( 'NONE',  ( 44.82050807568879947, -5.000000000000000000, -37.63139720814411504 ) ) ;
#7443 = AXIS2_PLACEMENT_3D ( 'NONE', #6699, #13047, #9282 ) ;
#7442 = DIRECTION ( 'NONE',  ( 0.000000000000000000, 0.000000000000000000, -1.000000000000000000 ) ) ;
#7444 = DIRECTION ( 'NONE',  ( 0.000000000000000000, -0.4999999999999993894, 0.8660254037844389297 ) ) ;
#7445 = LINE ( 'NONE', #9779, #1628 ) ;
#7446 = EDGE_CURVE ( 'NONE', #15896, #15795, #1905, .T. ) ;
#7447 = CARTESIAN_POINT ( 'NONE',  ( 3.152801135295367541, -24.56250000136559564, -3.152801135295367541 ) ) ;
#7448 = DIRECTION ( 'NONE',  ( 1.000000000000000000, -1.734723475976808080E-16, 0.000000000000000000 ) ) ;
#7449 = APPLICATION_CONTEXT ( 'automotive_design' ) ;
#7450 = DIRECTION ( 'NONE',  ( 0.000000000000000000, -1.000000000000000000, 0.000000000000000000 ) ) ;
#7451 = CARTESIAN_POINT ( 'NONE',  ( 3.535533905932738197, -30.00000000273118417, -3.535533905932738197 ) ) ;
#7452 = CARTESIAN_POINT ( 'NONE',  ( -9.184850993605147944E-16, -29.37500000273118417, 5.000000000000000000 ) ) ;
#7453 = CIRCLE ( 'NONE', #15191, 32.00000000000000000 ) ;
#7454 = CARTESIAN_POINT ( 'NONE',  ( 4.458734124999999437, -29.37500000136559208, -1.846868145590734978 ) ) ;
#7455 = ORIENTED_EDGE ( 'NONE', *, *, #1060, .F. ) ;
#7456 = SURFACE_STYLE_FILL_AREA ( #3718 ) ;
#7457 = VERTEX_POINT ( 'NONE', #13777 ) ;
#7458 = LINE ( 'NONE', #3477, #160 ) ;
#7459 = AXIS2_PLACEMENT_3D ( 'NONE', #11288, #2800, #11204 ) ;
#7460 = ORIENTED_EDGE ( 'NONE', *, *, #4218, .T. ) ;
#7461 = CARTESIAN_POINT ( 'NONE',  ( 10.17949192431126093, 0.000000000000000000, -57.63139720814412925 ) ) ;
#7462 = AXIS2_PLACEMENT_3D ( 'NONE', #2501, #3649, #13334 ) ;
#7463 = CARTESIAN_POINT ( 'NONE',  ( 40.62016163511525946, -3.061199086701585248, 27.37108366584844532 ) ) ;
#7464 = CARTESIAN_POINT ( 'NONE',  ( -3.916244202832140253, 2.131511515620587272, -3.937499998634404808 ) ) ;
#7465 = PRODUCT_CONTEXT ( 'NONE', #15891, 'mechanical' ) ;
#7466 = CIRCLE ( 'NONE', #8501, 2.500000000000000888 ) ;
#7467 = CARTESIAN_POINT ( 'NONE',  ( 4.276409079477644148, 1.261996585732577891, -5.562499998634406140 ) ) ;
#7468 = FACE_BOUND ( 'NONE', #6516, .T. ) ;
#7469 = DIRECTION ( 'NONE',  ( 0.000000000000000000, -0.5000000000000011102, -0.8660254037844379305 ) ) ;
#7470 = ORIENTED_EDGE ( 'NONE', *, *, #14817, .T. ) ;
#7471 = DIRECTION ( 'NONE',  ( 0.000000000000000000, 0.000000000000000000, 1.000000000000000000 ) ) ;
#7472 = VERTEX_POINT ( 'NONE', #13621 ) ;
#7473 = DIRECTION ( 'NONE',  ( 0.000000000000000000, 0.000000000000000000, 1.000000000000000000 ) ) ;
#7474 = CYLINDRICAL_SURFACE ( 'NONE', #949, 6.000000000000000888 ) ;
#7475 = ORIENTED_EDGE ( 'NONE', *, *, #3327, .F. ) ;
#7476 = CONTEXT_DEPENDENT_SHAPE_REPRESENTATION ( #13, #7394 ) ;
#7477 = CARTESIAN_POINT ( 'NONE',  ( -1.261996585732579224, 4.276409079477648589, -1.312499998634406140 ) ) ;
#7478 = EDGE_CURVE ( 'NONE', #11064, #2143, #12648, .T. ) ;
#7479 = CYLINDRICAL_SURFACE ( 'NONE', #8659, 9.999999999999980460 ) ;
#7480 = AXIS2_PLACEMENT_3D ( 'NONE', #1134, #5016, #12197 ) ;
#7481 = DIRECTION ( 'NONE',  ( 1.000000000000000000, 0.000000000000000000, 0.000000000000000000 ) ) ;
#7482 = DIRECTION ( 'NONE',  ( 0.000000000000000000, 0.000000000000000000, 1.000000000000000000 ) ) ;
#7483 = CARTESIAN_POINT ( 'NONE',  ( -31.74999999999995737, 0.000000000000000000, 0.000000000000000000 ) ) ;
#7484 = CARTESIAN_POINT ( 'NONE',  ( 5.381735091635035495, -0.5711823568785978633, -4.937499997268820273 ) ) ;
#7485 = LINE ( 'NONE', #6268, #1242 ) ;
#7486 = CARTESIAN_POINT ( 'NONE',  ( 47.32050807568880657, -5.000000000000000000, -41.96152422706630603 ) ) ;
#7487 = CARTESIAN_POINT ( 'NONE',  ( 4.458734124999999437, -27.62500000136559564, -1.846868145590734978 ) ) ;
#7488 = ORIENTED_EDGE ( 'NONE', *, *, #12350, .F. ) ;
#7489 = CARTESIAN_POINT ( 'NONE',  ( -1.846868145590737420, -22.75000000136559919, 4.458734124999997661 ) ) ;
#7490 = CARTESIAN_POINT ( 'NONE',  ( 4.799145180956616130, -0.5093500532425063732, -5.374999998634406140 ) ) ;
#7491 = FACE_OUTER_BOUND ( 'NONE', #15303, .T. ) ;
#7492 = ORIENTED_EDGE ( 'NONE', *, *, #673, .F. ) ;
#7493 = VERTEX_POINT ( 'NONE', #66 ) ;
#7494 =( BOUNDED_CURVE ( )  B_SPLINE_CURVE ( 2, ( #6591, #6683, #3026, #5535, #10470, #11505, #376, #14013, #9182 ),
 .UNSPECIFIED., .F., .F. ) 
 B_SPLINE_CURVE_WITH_KNOTS ( ( 3, 2, 2, 2, 3 ),
 ( 0.4250000000000000444, 0.4375000000000000555, 0.4500000000000000666, 0.4625000000000001332, 0.4750000000000000888 ),
 .UNSPECIFIED. ) 
 CURVE ( )  GEOMETRIC_REPRESENTATION_ITEM ( )  RATIONAL_B_SPLINE_CURVE ( ( 0.9999999999999996669, 0.9238795325112870716, 1.000000000000000000, 0.9238795325112867385, 1.000000000000000000, 0.9238795325112867385, 1.000000000000000000, 0.9238795325112860723, 1.000000000000000666 ) ) 
 REPRESENTATION_ITEM ( '' )  );
#7495 = SHAPE_REPRESENTATION ( 'Drive Unit', ( #3223 ), #15660 ) ;
#7496 = FILL_AREA_STYLE ('',( #2625 ) ) ;
#7497 = ORIENTED_EDGE ( 'NONE', *, *, #13177, .T. ) ;
#7498 = CARTESIAN_POINT ( 'NONE',  ( 5.000000000000000888, -31.06250000273118772, -2.071067811865475505 ) ) ;
#7499 = EDGE_CURVE ( 'NONE', #5431, #9125, #7756, .T. ) ;
#7500 = CARTESIAN_POINT ( 'NONE',  ( 4.458734124999999437, -21.56250000136559208, 0.000000000000000000 ) ) ;
#7501 = EDGE_CURVE ( 'NONE', #4500, #13155, #15173, .T. ) ;
#7502 = DIRECTION ( 'NONE',  ( -0.000000000000000000, -1.000000000000000000, -0.000000000000000000 ) ) ;
#7503 = LINE ( 'NONE', #7581, #4561 ) ;
#7504 = CARTESIAN_POINT ( 'NONE',  ( 4.387887813791333080, -3.660959011663040386, 48.61734447228085543 ) ) ;
#7505 = DIRECTION ( 'NONE',  ( -0.000000000000000000, -1.000000000000000000, -0.000000000000000000 ) ) ;
#7506 = CARTESIAN_POINT ( 'NONE',  ( -3.401574460001764777, 4.209348295687701302, -1.687500000000002442 ) ) ;
#7507 = CARTESIAN_POINT ( 'NONE',  ( 4.209348295687701302, 3.401574460001766109, -3.937500000000000888 ) ) ;
#7508 = DIRECTION ( 'NONE',  ( 0.000000000000000000, 0.000000000000000000, 1.000000000000000000 ) ) ;
#7509 = CARTESIAN_POINT ( 'NONE',  ( 4.458734124999999437, -27.43750000136559564, 0.000000000000000000 ) ) ;
#7510 = CARTESIAN_POINT ( 'NONE',  ( 2.131511515620586383, 3.916244202832140253, -2.437499998634407028 ) ) ;
#7511 = ORIENTED_EDGE ( 'NONE', *, *, #9325, .F. ) ;
#7512 = DIRECTION ( 'NONE',  ( 0.000000000000000000, 1.000000000000000000, 0.000000000000000000 ) ) ;
#7513 = ORIENTED_EDGE ( 'NONE', *, *, #9158, .T. ) ;
#7514 = EDGE_LOOP ( 'NONE', ( #14519, #13033, #11454, #377 ) ) ;
#7515 = CARTESIAN_POINT ( 'NONE',  ( 4.458734124999998549, -3.052311964297492742E-11, -0.3789984458506765463 ) ) ;
#7516 = CARTESIAN_POINT ( 'NONE',  ( 2.730187237215162345E-16, -25.18750000136559564, -4.458734124999999437 ) ) ;
#7517 = EDGE_CURVE ( 'NONE', #13173, #2847, #5156, .T. ) ;
#7518 = CARTESIAN_POINT ( 'NONE',  ( -28.86751345948129455, -37.00000000000000711, 20.00000000000000355 ) ) ;
#7519 = EDGE_CURVE ( 'NONE', #757, #794, #2712, .T. ) ;
#7520 = ORIENTED_EDGE ( 'NONE', *, *, #10845, .T. ) ;
#7521 = FACE_OUTER_BOUND ( 'NONE', #15343, .T. ) ;
#7522 = PLANE ( 'NONE',  #13123 ) ;
#7523 = CARTESIAN_POINT ( 'NONE',  ( -3.033343224707664820, 3.753672977998667726, -2.999999998634409248 ) ) ;
#7524 = CYLINDRICAL_SURFACE ( 'NONE', #10150, 2.500000000000000444 ) ;
#7525 = CARTESIAN_POINT ( 'NONE',  ( 2.071067811865476394, -30.18750000000000711, 5.000000000000000000 ) ) ;
#7526 = CARTESIAN_POINT ( 'NONE',  ( -5.000000000000004441, -1.011557177027151181E-15, -4.420263044861760804 ) ) ;
#7527 = LINE ( 'NONE', #4194, #14912 ) ;
#7528 = CARTESIAN_POINT ( 'NONE',  ( -5.000000000000000888, -26.56250000273118417, 2.071067811865474617 ) ) ;
#7529 = B_SPLINE_CURVE_WITH_KNOTS ( 'NONE', 3,
 ( #3036, #1819, #5545, #3121, #13039, #1980, #6925, #8062, #12960, #13124 ),
 .UNSPECIFIED., .F., .F.,
 ( 4, 2, 2, 2, 4 ),
 ( 0.01051144076094935077, 0.01162027323572611091, 0.01272910571050287105, 0.01383793818527963120, 0.01494677066005639134 ),
 .UNSPECIFIED. ) ;
#7530 = CARTESIAN_POINT ( 'NONE',  ( 4.391654775818395251, -2.390265326283149694, -5.999999997268814944 ) ) ;
#7531 = CARTESIAN_POINT ( 'NONE',  ( 4.458734124999999437, -29.43750000136559208, 0.000000000000000000 ) ) ;
#7532 = DIRECTION ( 'NONE',  ( 0.000000000000000000, -1.000000000000000000, 0.000000000000000000 ) ) ;
#7533 = ORIENTED_EDGE ( 'NONE', *, *, #15514, .T. ) ;
#7534 = ORIENTED_EDGE ( 'NONE', *, *, #3560, .F. ) ;
#7535 = PRODUCT_DEFINITION_SHAPE ( 'NONE', 'NONE',  #15988 ) ;
#7536 = FILL_AREA_STYLE ('',( #2664 ) ) ;
#7538 = EDGE_CURVE ( 'NONE', #9091, #307, #11125, .T. ) ;
#7537 = ORIENTED_EDGE ( 'NONE', *, *, #10397, .F. ) ;
#7539 = CARTESIAN_POINT ( 'NONE',  ( 45.58845726811992449, -5.000000000000004441, -42.96152422706630603 ) ) ;
#7540 = ADVANCED_FACE ( 'NONE', ( #10087 ), #388, .F. ) ;
#7541 = ORIENTED_EDGE ( 'NONE', *, *, #11026, .T. ) ;
#7542 = CARTESIAN_POINT ( 'NONE',  ( 9.999999999999891642, -13.00000000000000178, -17.32050807568883499 ) ) ;
#7543 = CARTESIAN_POINT ( 'NONE',  ( -5.000000000000095035, -0.7223674278660573433, -4.396799362785971610 ) ) ;
#7544 = CARTESIAN_POINT ( 'NONE',  ( 3.916244202832140253, -2.131511515620588160, -4.437499998634405252 ) ) ;
#7545 = VECTOR ( 'NONE', #9080, 1000.000000000000000 ) ;
#7546 = APPLICATION_PROTOCOL_DEFINITION ( 'draft international standard', 'automotive_design', 1998, #7449 ) ;
#7547 = CARTESIAN_POINT ( 'NONE',  ( 3.033343224707661712, -3.753672977998669946, -6.749999998634408804 ) ) ;
#7548 = FACE_BOUND ( 'NONE', #14813, .T. ) ;
#7549 = CARTESIAN_POINT ( 'NONE',  ( 3.061616997868383141E-16, -23.75000000000000000, -5.000000000000000000 ) ) ;
#7550 = VERTEX_POINT ( 'NONE', #1340 ) ;
#7551 = CARTESIAN_POINT ( 'NONE',  ( -7.500000000000005329, 3.608439182435162262, -7.298562697733104621 ) ) ;
#7552 = VERTEX_POINT ( 'NONE', #12329 ) ;
#7553 = CARTESIAN_POINT ( 'NONE',  ( -28.86751345948130165, 0.000000000000000000, 20.00000000000000355 ) ) ;
#7554 = CARTESIAN_POINT ( 'NONE',  ( -41.99999999999978684, -9.000000000000001776, -1.500000000000000888 ) ) ;
#7555 = EDGE_CURVE ( 'NONE', #1929, #11041, #8715, .T. ) ;
#7556 = ORIENTED_EDGE ( 'NONE', *, *, #9426, .T. ) ;
#7557 = ITEM_DEFINED_TRANSFORMATION ( 'NONE', 'NONE', #4769,  #3223 ) ;
#7558 = CARTESIAN_POINT ( 'NONE',  ( -3.753672977998669502, -3.033343224707661712, -6.999999998634409692 ) ) ;
#7559 = FILL_AREA_STYLE ('',( #11105 ) ) ;
#7560 = AXIS2_PLACEMENT_3D ( 'NONE', #15591, #9298, #3141 ) ;
#7561 = CARTESIAN_POINT ( 'NONE',  ( -0.5093500532425060401, -4.799145180956616130, -7.624999998634407916 ) ) ;
#7562 = DIRECTION ( 'NONE',  ( 0.000000000000000000, -1.000000000000000000, 0.000000000000000000 ) ) ;
#7563 = PRODUCT_DEFINITION_CONTEXT ( 'detailed design', #1125, 'design' ) ;
#7564 = DIRECTION ( 'NONE',  ( -0.5000000000000005551, 0.000000000000000000, 0.8660254037844382635 ) ) ;
#7565 = CARTESIAN_POINT ( 'NONE',  ( -3.401574460001764777, 4.209348295687701302, -2.562499997268814944 ) ) ;
#7566 = DIRECTION ( 'NONE',  ( 0.000000000000000000, 1.000000000000000000, 0.000000000000000000 ) ) ;
#7567 = ADVANCED_FACE ( 'NONE', ( #11365 ), #3067, .T. ) ;
#7568 = CARTESIAN_POINT ( 'NONE',  ( 3.535533905932736864, -28.25000000273118772, 3.535533905932738641 ) ) ;
#7569 = CARTESIAN_POINT ( 'NONE',  ( -3.152801135295367096, -25.31250000136559564, -3.152801135295367541 ) ) ;
#7570 = ORIENTED_EDGE ( 'NONE', *, *, #9644, .F. ) ;
#7571 = FACE_OUTER_BOUND ( 'NONE', #393, .T. ) ;
#7572 = CARTESIAN_POINT ( 'NONE',  ( 4.799145180956616130, -0.5093500532425063732, -7.374999998634408804 ) ) ;
#7573 = AXIS2_PLACEMENT_3D ( 'NONE', #9067, #13969, #340 ) ;
#7574 = FACE_OUTER_BOUND ( 'NONE', #1040, .T. ) ;
#7575 = ORIENTED_EDGE ( 'NONE', *, *, #1179, .T. ) ;
#7576 = ORIENTED_EDGE ( 'NONE', *, *, #6987, .T. ) ;
#7577 = ORIENTED_EDGE ( 'NONE', *, *, #15764, .T. ) ;
#7578 = CARTESIAN_POINT ( 'NONE',  ( 3.152801135295366208, -21.81250000136559208, 3.152801135295367985 ) ) ;
#7579 = CARTESIAN_POINT ( 'NONE',  ( 0.000000000000000000, -20.00000000000000000, 0.000000000000000000 ) ) ;
#7580 = DIRECTION ( 'NONE',  ( 0.000000000000000000, 0.000000000000000000, -1.000000000000000000 ) ) ;
#7581 = CARTESIAN_POINT ( 'NONE',  ( -2.500000000000000888, 0.000000000000000000, -4.974599999999998801 ) ) ;
#7582 = CARTESIAN_POINT ( 'NONE',  ( -1.282512619719235580, -8.391164935524143331, -7.795653906408909428 ) ) ;
#7583 = CARTESIAN_POINT ( 'NONE',  ( 0.000000000000000000, 0.000000000000000000, -8.499999999999996447 ) ) ;
#7584 = CARTESIAN_POINT ( 'NONE',  ( -1.415196051561583790, 4.795541693661363958, -3.750000000000000000 ) ) ;
#7585 = CARTESIAN_POINT ( 'NONE',  ( -54.99999999999999289, -25.00000000000000000, -17.50000000000000000 ) ) ;
#7586 = EDGE_CURVE ( 'NONE', #11426, #1698, #3928, .T. ) ;
#7587 = CARTESIAN_POINT ( 'NONE',  ( 3.061616997868383141E-16, -28.75000000000000000, -5.000000000000000000 ) ) ;
#7588 = ADVANCED_FACE ( 'NONE', ( #317 ), #15258, .F. ) ;
#7589 = CARTESIAN_POINT ( 'NONE',  ( -3.152801135295367096, -28.06250000136559564, -3.152801135295367541 ) ) ;
#7590 =( BOUNDED_CURVE ( )  B_SPLINE_CURVE ( 2, ( #3772, #11056, #1268, #8403, #11206, #8482, #14608, #68, #1185, #6213, #8561 ),
 .UNSPECIFIED., .F., .F. ) 
 B_SPLINE_CURVE_WITH_KNOTS ( ( 3, 2, 2, 2, 2, 3 ),
 ( 0.3045872658012772627, 0.3125000000000000000, 0.3250000000000000111, 0.3375000000000000222, 0.3499999999999999778, 0.3545872658012772516 ),
 .UNSPECIFIED. ) 
 CURVE ( )  GEOMETRIC_REPRESENTATION_ITEM ( )  RATIONAL_B_SPLINE_CURVE ( ( 0.9646335149384808183, 0.9518143178943437865, 1.000000000000000000, 0.9238795325112867385, 1.000000000000000000, 0.9238795325112867385, 1.000000000000000000, 0.9238795325112867385, 1.000000000000000000, 0.9720652146169430630, 0.9646335149384808183 ) ) 
 REPRESENTATION_ITEM ( '' )  );
#7591 = CARTESIAN_POINT ( 'NONE',  ( -4.276409079477644148, -1.261996585732578335, -3.062499998634407472 ) ) ;
#7592 = ORIENTED_EDGE ( 'NONE', *, *, #3648, .F. ) ;
#7593 = DIRECTION ( 'NONE',  ( 0.000000000000000000, 0.000000000000000000, -1.000000000000000000 ) ) ;
#7594 = EDGE_LOOP ( 'NONE', ( #4407, #12194, #10051 ) ) ;
#7595 = ORIENTED_EDGE ( 'NONE', *, *, #10842, .T. ) ;
#7596 = CARTESIAN_POINT ( 'NONE',  ( 3.152801135295367541, -24.31250000136559564, -3.152801135295367541 ) ) ;
#7597 = CARTESIAN_POINT ( 'NONE',  ( -7.500000000000000000, -4.330127018922196314, -9.999999999999998224 ) ) ;
#7598 = VECTOR ( 'NONE', #4473, 1000.000000000000114 ) ;
#7599 = ORIENTED_EDGE ( 'NONE', *, *, #10570, .F. ) ;
#7600 = CARTESIAN_POINT ( 'NONE',  ( -4.000000000000000000, -2.309401076758515803, -0.4999999999999995559 ) ) ;
#7601 = FACE_BOUND ( 'NONE', #2862, .T. ) ;
#7602 = CARTESIAN_POINT ( 'NONE',  ( 4.276409079477644148, 1.261996585732577891, -1.312499998634406140 ) ) ;
#7603 = DIRECTION ( 'NONE',  ( -0.000000000000000000, 1.000000000000000000, -0.000000000000000000 ) ) ;
#7604 = CARTESIAN_POINT ( 'NONE',  ( -9.184850993605147944E-16, -29.25000000000000000, 5.000000000000000000 ) ) ;
#7605 = CARTESIAN_POINT ( 'NONE',  ( 2.500000000000000000, 0.000000000000000000, 2.041999999999999815 ) ) ;
#7606 = CARTESIAN_POINT ( 'NONE',  ( -35.00000000000000000, 37.00000000000000000, -2.649999999999985700 ) ) ;
#7607 = ADVANCED_FACE ( 'NONE', ( #12724 ), #13945, .T. ) ;
#7608 = CARTESIAN_POINT ( 'NONE',  ( 5.000000000000000888, -30.06250000273118417, -2.071067811865475505 ) ) ;
#7609 = CARTESIAN_POINT ( 'NONE',  ( 4.999999999999845457, -1.272547481429021854, -3.086597482644650281 ) ) ;
#7610 = COLOUR_RGB ( '', 0.31764706, 0.68627451, 0.89019608) ;
#7611 = CARTESIAN_POINT ( 'NONE',  ( -1.846868145590737420, -29.75000000136559564, 4.458734124999997661 ) ) ;
#7612 = PRESENTATION_STYLE_ASSIGNMENT (( #5182 ) ) ;
#7613 = ORIENTED_EDGE ( 'NONE', *, *, #13802, .T. ) ;
#7614 = ORIENTED_EDGE ( 'NONE', *, *, #12797, .F. ) ;
#7615 = AXIS2_PLACEMENT_3D ( 'NONE', #13623, #13295, #9670 ) ;
#7616 = ORIENTED_EDGE ( 'NONE', *, *, #8377, .F. ) ;
#7617 = DIRECTION ( 'NONE',  ( -1.000000000000000000, 0.000000000000000000, 0.000000000000000000 ) ) ;
#7618 = EDGE_LOOP ( 'NONE', ( #6795, #6642, #9515, #9455 ) ) ;
#7619 = FACE_OUTER_BOUND ( 'NONE', #5682, .T. ) ;
#7620 =( GEOMETRIC_REPRESENTATION_CONTEXT ( 3 ) GLOBAL_UNCERTAINTY_ASSIGNED_CONTEXT ( ( #6265 ) ) GLOBAL_UNIT_ASSIGNED_CONTEXT ( ( #7179, #11848, #15749 ) ) REPRESENTATION_CONTEXT ( 'NONE', 'WORKASPACE' ) );
#7621 = CARTESIAN_POINT ( 'NONE',  ( -9.184850993605147944E-16, -31.25000000000000000, 5.000000000000000000 ) ) ;
#7622 = AXIS2_PLACEMENT_3D ( 'NONE', #6208, #12161, #13211 ) ;
#7623 = CARTESIAN_POINT ( 'NONE',  ( 0.000000000000000000, -20.00000000000000000, 5.000000000000000000 ) ) ;
#7624 = EDGE_CURVE ( 'NONE', #10386, #10448, #12230, .T. ) ;
#7625 = B_SPLINE_CURVE_WITH_KNOTS ( 'NONE', 3,
 ( #2068, #11756, #2956, #7012, #474, #632 ),
 .UNSPECIFIED., .F., .F.,
 ( 4, 2, 4 ),
 ( 0.004444412883774351460, 0.006655097293744442408, 0.008865781703714532488 ),
 .UNSPECIFIED. ) ;
#7626 = EDGE_CURVE ( 'NONE', #10782, #5482, #4874, .T. ) ;
#7627 = EDGE_CURVE ( 'NONE', #4627, #3387, #1823, .T. ) ;
#7628 = DIRECTION ( 'NONE',  ( -6.123233995736766036E-17, -1.000000000000000000, -4.275831445896958607E-31 ) ) ;
#7629 = EDGE_CURVE ( 'NONE', #11803, #4563, #15353, .T. ) ;
#7630 = CARTESIAN_POINT ( 'NONE',  ( -3.916244202832140253, 2.131511515620587272, -7.187499998634407916 ) ) ;
#7631 = CARTESIAN_POINT ( 'NONE',  ( 35.00000000000000000, 37.00000000000000000, -5.999999999999991118 ) ) ;
#7632 = CARTESIAN_POINT ( 'NONE',  ( 0.000000000000000000, 40.00000000000000000, 0.000000000000000000 ) ) ;
#7633 = ORIENTED_EDGE ( 'NONE', *, *, #4427, .F. ) ;
#7634 = CARTESIAN_POINT ( 'NONE',  ( 3.393972966170744510, -3.061199086701537286, -48.86363371475460582 ) ) ;
#7635 = CIRCLE ( 'NONE', #7884, 5.000000000000000000 ) ;
#7636 = ORIENTED_EDGE ( 'NONE', *, *, #6961, .T. ) ;
#7637 = CARTESIAN_POINT ( 'NONE',  ( 0.000000000000000000, 0.000000000000000000, -4.000000000000000000 ) ) ;
#7638 = CARTESIAN_POINT ( 'NONE',  ( 67.49999999999931788, 40.00000000000000000, 2.081668171172168513E-14 ) ) ;
#7639 = CIRCLE ( 'NONE', #13526, 2.055000000000000160 ) ;
#7640 = ORIENTED_EDGE ( 'NONE', *, *, #13097, .F. ) ;
#7641 = ITEM_DEFINED_TRANSFORMATION ( 'NONE', 'NONE', #4504,  #3223 ) ;
#7642 = CARTESIAN_POINT ( 'NONE',  ( 3.916244202832140253, -2.131511515620588160, -5.687499998634406140 ) ) ;
#7643 = CARTESIAN_POINT ( 'NONE',  ( 5.000000000000093259, 0.7223674278660628945, -4.896799362785971610 ) ) ;
#7644 = COLOUR_RGB ( '', 0.09019608, 0.27058824, 0.51372549) ;
#7645 = DIRECTION ( 'NONE',  ( -0.000000000000000000, 1.000000000000000000, -0.000000000000000000 ) ) ;
#7646 = CARTESIAN_POINT ( 'NONE',  ( -45.00000000000000000, 0.000000000000000000, -7.500000000000000000 ) ) ;
#7647 = VECTOR ( 'NONE', #14972, 1000.000000000000114 ) ;
#7648 = ADVANCED_FACE ( 'NONE', ( #469 ), #7989, .F. ) ;
#7649 = FACE_BOUND ( 'NONE', #7255, .T. ) ;
#7650 = CIRCLE ( 'NONE', #1138, 5.000000000000000000 ) ;
#7651 = CARTESIAN_POINT ( 'NONE',  ( 0.5711823568785989735, 5.381735091635026613, -5.687499997268815832 ) ) ;
#7652 = CARTESIAN_POINT ( 'NONE',  ( -91.33974596215560382, -110.0591436588189396, -7.500000000000001776 ) ) ;
#7653 = DIRECTION ( 'NONE',  ( 0.000000000000000000, 0.000000000000000000, 1.000000000000000000 ) ) ;
#7654 = DIRECTION ( 'NONE',  ( -1.387778780781446464E-15, -1.000000000000000000, 1.387778780781445478E-15 ) ) ;
#7655 = ORIENTED_EDGE ( 'NONE', *, *, #1280, .T. ) ;
#7656 = LINE ( 'NONE', #3990, #6667 ) ;
#7657 = CARTESIAN_POINT ( 'NONE',  ( -4.207491450040567571, 2.029819825146470524, -3.671670828759566074 ) ) ;
#7658 = CARTESIAN_POINT ( 'NONE',  ( 0.000000000000000000, 50.00000000000000000, 0.000000000000000000 ) ) ;
#7659 = ORIENTED_EDGE ( 'NONE', *, *, #3719, .F. ) ;
#7660 = ORIENTED_EDGE ( 'NONE', *, *, #10590, .F. ) ;
#7661 = ORIENTED_EDGE ( 'NONE', *, *, #7074, .F. ) ;
#7662 = CARTESIAN_POINT ( 'NONE',  ( -17.99999999999979394, -11.00000000000000178, -3.500000000000000888 ) ) ;
#7663 = DIRECTION ( 'NONE',  ( 0.000000000000000000, 0.000000000000000000, 1.000000000000000000 ) ) ;
#7664 = AXIS2_PLACEMENT_3D ( 'NONE', #5238, #486, #6302 ) ;
#7665 = CARTESIAN_POINT ( 'NONE',  ( 3.061616997868383141E-16, -25.75000000000000355, -5.000000000000000000 ) ) ;
#7666 = DIRECTION ( 'NONE',  ( -0.000000000000000000, -1.000000000000000000, -0.000000000000000000 ) ) ;
#7668 = DIRECTION ( 'NONE',  ( 0.000000000000000000, 0.000000000000000000, -1.000000000000000000 ) ) ;
#7667 = AXIS2_PLACEMENT_3D ( 'NONE', #432, #356, #6494 ) ;
#7669 = DIRECTION ( 'NONE',  ( 0.000000000000000000, 1.000000000000000000, -1.471414886128461471E-15 ) ) ;
#7670 = PRODUCT_DEFINITION_SHAPE ( 'NONE', 'NONE',  #15999 ) ;
#7671 = CARTESIAN_POINT ( 'NONE',  ( 3.401574460001763001, -4.209348295687703967, -6.187500000000003553 ) ) ;
#7672 = CARTESIAN_POINT ( 'NONE',  ( -3.401574460001765221, 4.209348295687701302, -2.687500000000002665 ) ) ;
#7673 = DIRECTION ( 'NONE',  ( -1.000000000000000000, 0.000000000000000000, 0.000000000000000000 ) ) ;
#7674 = CARTESIAN_POINT ( 'NONE',  ( 1.846868145590735200, -22.25000000136559564, -4.458734125000000326 ) ) ;
#7675 = CARTESIAN_POINT ( 'NONE',  ( 4.276409079477644148, 1.261996585732577891, -7.562499998634407916 ) ) ;
#7676 = EDGE_LOOP ( 'NONE', ( #7234, #1332, #7871, #5216 ) ) ;
#7677 = CARTESIAN_POINT ( 'NONE',  ( -7.500000000000006217, -2.930060224340423680, -0.4701183149080278012 ) ) ;
#7678 = ORIENTED_EDGE ( 'NONE', *, *, #13885, .F. ) ;
#7679 = ORIENTED_EDGE ( 'NONE', *, *, #10064, .T. ) ;
#7680 = CARTESIAN_POINT ( 'NONE',  ( 2.730187237215162345E-16, -30.43750000136559564, -4.458734124999999437 ) ) ;
#7681 = LINE ( 'NONE', #10015, #15649 ) ;
#7682 = AXIS2_PLACEMENT_3D ( 'NONE', #6367, #6287, #7824 ) ;
#7683 = ORIENTED_EDGE ( 'NONE', *, *, #10414, .T. ) ;
#7684 = CARTESIAN_POINT ( 'NONE',  ( -4.000000000000000000, -0.3979232138631226823, -3.896351557369779711E-17 ) ) ;
#7685 = ADVANCED_FACE ( 'NONE', ( #6768 ), #12888, .T. ) ;
#7686 = EDGE_CURVE ( 'NONE', #8590, #10453, #3829, .T. ) ;
#7687 = EDGE_CURVE ( 'NONE', #794, #11044, #8297, .T. ) ;
#7688 = CIRCLE ( 'NONE', #9994, 31.99999999999999289 ) ;
#7689 = DIRECTION ( 'NONE',  ( -1.000000000000000000, -1.541976423090495140E-16, 0.000000000000000000 ) ) ;
#7690 = CARTESIAN_POINT ( 'NONE',  ( -4.799145180956616130, 0.5093500532425063732, -0.8749999986344056957 ) ) ;
#7691 = FACE_OUTER_BOUND ( 'NONE', #4883, .T. ) ;
#7692 = CARTESIAN_POINT ( 'NONE',  ( 3.535533905932736864, -28.12500000000000000, 3.535533905932738641 ) ) ;
#7693 = CARTESIAN_POINT ( 'NONE',  ( -44.41942919302233150, -4.462727778340706664, -20.05540692447297246 ) ) ;
#7694 = TOROIDAL_SURFACE ( 'NONE', #2766, 2.700000000000000622, 0.2000000000000000111 ) ;
#7695 = DIRECTION ( 'NONE',  ( 0.000000000000000000, 0.000000000000000000, -1.000000000000000000 ) ) ;
#7696 = CARTESIAN_POINT ( 'NONE',  ( 5.000000000000000000, -27.12500000273118772, 0.000000000000000000 ) ) ;
#7697 = DIRECTION ( 'NONE',  ( -0.000000000000000000, -1.000000000000000000, -0.000000000000000000 ) ) ;
#7698 = CARTESIAN_POINT ( 'NONE',  ( 2.071067811865462183, -24.31250000273118417, 5.000000000000013323 ) ) ;
#7699 = CARTESIAN_POINT ( 'NONE',  ( -21.01110699893041556, 0.000000000000000000, -36.39230484541334221 ) ) ;
#7700 = EDGE_LOOP ( 'NONE', ( #9183, #12344, #13282, #8830 ) ) ;
#7701 = VERTEX_POINT ( 'NONE', #15572 ) ;
#7702 = VECTOR ( 'NONE', #5748, 1000.000000000000000 ) ;
#7703 = VERTEX_POINT ( 'NONE', #11753 ) ;
#7704 = CARTESIAN_POINT ( 'NONE',  ( -44.37850886472753587, -4.098233149438287093, 20.20989737819990495 ) ) ;
#7705 = ORIENTED_EDGE ( 'NONE', *, *, #13235, .T. ) ;
#7706 = DIRECTION ( 'NONE',  ( -0.000000000000000000, 1.000000000000000000, -0.000000000000000000 ) ) ;
#7707 = AXIS2_PLACEMENT_3D ( 'NONE', #15447, #15359, #15678 ) ;
#7708 = EDGE_CURVE ( 'NONE', #1994, #5239, #10332, .T. ) ;
#7709 = ADVANCED_FACE ( 'NONE', ( #7904 ), #5470, .F. ) ;
#7710 = PRODUCT_RELATED_PRODUCT_CATEGORY ( 'part', '', ( #10551 ) ) ;
#7711 = CARTESIAN_POINT ( 'NONE',  ( -2.071067811865469288, -31.31250000000000000, 5.000000000000007994 ) ) ;
#7712 = CARTESIAN_POINT ( 'NONE',  ( -4.458734125000000326, -31.25000000136559564, -1.846868145590735644 ) ) ;
#7713 = VECTOR ( 'NONE', #9878, 1000.000000000000000 ) ;
#7714 = PRODUCT_CONTEXT ( 'NONE', #4842, 'mechanical' ) ;
#7715 = CARTESIAN_POINT ( 'NONE',  ( 2.131511515620586383, 3.916244202832140253, -7.437499998634407916 ) ) ;
#7716 = CARTESIAN_POINT ( 'NONE',  ( 4.211140560182196957, 2.431303136016536470, -3.745885042887433514 ) ) ;
#7717 = VECTOR ( 'NONE', #10890, 1000.000000000000000 ) ;
#7718 = EDGE_LOOP ( 'NONE', ( #13394, #5260, #9602, #6918, #11759 ) ) ;
#7719 = CARTESIAN_POINT ( 'NONE',  ( -5.000000000000004441, -1.011557177027151181E-15, -5.420263044861760804 ) ) ;
#7720 = STYLED_ITEM ( 'NONE', ( #7810 ), #9346 ) ;
#7721 = SHAPE_REPRESENTATION_RELATIONSHIP ( 'NONE' , 'NONE' ,  #6981, #1740 ) ;
#7722 = VERTEX_POINT ( 'NONE', #15418 ) ;
#7723 = DIRECTION ( 'NONE',  ( 0.000000000000000000, 0.000000000000000000, -1.000000000000000000 ) ) ;
#7724 = DIRECTION ( 'NONE',  ( -0.000000000000000000, -1.000000000000000000, -0.000000000000000000 ) ) ;
#7725 = AXIS2_PLACEMENT_3D ( 'NONE', #5525, #11810, #2040 ) ;
#7726 = ORIENTED_EDGE ( 'NONE', *, *, #10314, .T. ) ;
#7727 = CARTESIAN_POINT ( 'NONE',  ( 3.033343224707661712, -3.753672977998669502, -6.749999998634408804 ) ) ;
#7728 = EDGE_CURVE ( 'NONE', #9639, #14899, #11073, .T. ) ;
#7729 = EDGE_CURVE ( 'NONE', #11572, #10095, #11809, .T. ) ;
#7730 = SURFACE_SIDE_STYLE ('',( #12539 ) ) ;
#7731 = VECTOR ( 'NONE', #5947, 1000.000000000000000 ) ;
#7732 = AXIS2_PLACEMENT_3D ( 'NONE', #13794, #10268, #8651 ) ;
#7733 = DIRECTION ( 'NONE',  ( 1.000000000000000000, 0.000000000000000000, 0.000000000000000000 ) ) ;
#7734 = CARTESIAN_POINT ( 'NONE',  ( 5.000000000000000000, -21.12500000273118772, 0.000000000000000000 ) ) ;
#7735 = PLANE ( 'NONE',  #492 ) ;
#7736 = VECTOR ( 'NONE', #2235, 1000.000000000000000 ) ;
#7737 = CARTESIAN_POINT ( 'NONE',  ( 0.5711823568785989735, 5.381735091635026613, -3.687499997268817609 ) ) ;
#7738 = CARTESIAN_POINT ( 'NONE',  ( 4.000000000000000000, -2.309401076758514915, -3.433295621305383349 ) ) ;
#7739 = DIRECTION ( 'NONE',  ( -0.000000000000000000, -0.000000000000000000, 1.000000000000000000 ) ) ;
#7740 = DIRECTION ( 'NONE',  ( 0.000000000000000000, 0.000000000000000000, -1.000000000000000000 ) ) ;
#7741 = ORIENTED_EDGE ( 'NONE', *, *, #5062, .T. ) ;
#7742 = CARTESIAN_POINT ( 'NONE',  ( 0.000000000000000000, 0.000000000000000000, 0.000000000000000000 ) ) ;
#7743 = CARTESIAN_POINT ( 'NONE',  ( -3.033343224707664376, 3.753672977998667726, -7.999999998634409692 ) ) ;
#7744 = LINE ( 'NONE', #15161, #6360 ) ;
#7745 = ORIENTED_EDGE ( 'NONE', *, *, #1953, .T. ) ;
#7746 = ORIENTED_EDGE ( 'NONE', *, *, #13822, .T. ) ;
#7747 = EDGE_LOOP ( 'NONE', ( #12577, #11397, #14479, #6852, #12415 ) ) ;
#7748 = VECTOR ( 'NONE', #5681, 1000.000000000000000 ) ;
#7749 = CARTESIAN_POINT ( 'NONE',  ( -5.000000000000000888, 6.123233995736767268E-16, -25.03750572909317285 ) ) ;
#7750 = CARTESIAN_POINT ( 'NONE',  ( 2.500000000000000000, -1.178949249685213863, 2.042000000000002924 ) ) ;
#7751 = EDGE_CURVE ( 'NONE', #14753, #15272, #14210, .T. ) ;
#7752 = ADVANCED_BREP_SHAPE_REPRESENTATION ( '', ( #14042, #3223 ), #15084 ) ;
#7753 = DIRECTION ( 'NONE',  ( -0.000000000000000000, -1.000000000000000000, -0.000000000000000000 ) ) ;
#7754 = CARTESIAN_POINT ( 'NONE',  ( -8.673617379884035472E-16, -9.147862274876560562, -8.047472243342939535 ) ) ;
#7755 = CARTESIAN_POINT ( 'NONE',  ( 0.000000000000000000, 40.00000000000000000, -60.00000000000000000 ) ) ;
#7756 = LINE ( 'NONE', #2464, #10309 ) ;
#7757 = EDGE_CURVE ( 'NONE', #7238, #7869, #1014, .T. ) ;
#7758 = CARTESIAN_POINT ( 'NONE',  ( 1.415196051561583790, -4.795541693661363958, -5.250000000000000888 ) ) ;
#7759 = CARTESIAN_POINT ( 'NONE',  ( 3.535533905932736864, -30.12500000000000000, 3.535533905932738641 ) ) ;
#7760 = CARTESIAN_POINT ( 'NONE',  ( 5.000000000000000000, -29.00000000000000000, 0.000000000000000000 ) ) ;
#7761 = CARTESIAN_POINT ( 'NONE',  ( 3.152801135295367541, -23.31250000136559564, -3.152801135295367541 ) ) ;
#7762 = CARTESIAN_POINT ( 'NONE',  ( -4.799145180956616130, 0.5093500532425063732, -7.124999998634407916 ) ) ;
#7763 = EDGE_LOOP ( 'NONE', ( #11409, #14077, #7199, #2057 ) ) ;
#7764 = CARTESIAN_POINT ( 'NONE',  ( -2.720782245279947563E-14, 8.716839668575689259, -7.700121441565839220 ) ) ;
#7765 = ORIENTED_EDGE ( 'NONE', *, *, #6938, .F. ) ;
#7766 = ORIENTED_EDGE ( 'NONE', *, *, #2044, .F. ) ;
#7767 =( REPRESENTATION_RELATIONSHIP ('NONE','NONE', #4176, #790 ) REPRESENTATION_RELATIONSHIP_WITH_TRANSFORMATION ( #13588 )SHAPE_REPRESENTATION_RELATIONSHIP( ) );
#7768 = CARTESIAN_POINT ( 'NONE',  ( -1.846868145590737420, -22.75000000136559208, 4.458734124999999437 ) ) ;
#7769 = CARTESIAN_POINT ( 'NONE',  ( 4.769696007084728073, -13.00000000000000178, -1.500000000000000000 ) ) ;
#7770 = VERTEX_POINT ( 'NONE', #11911 ) ;
#7771 = CARTESIAN_POINT ( 'NONE',  ( -2.071067811865468400, -28.68750000000000000, -5.000000000000007994 ) ) ;
#7772 = FACE_OUTER_BOUND ( 'NONE', #11213, .T. ) ;
#7773 = LINE ( 'NONE', #15105, #10799 ) ;
#7774 = FACE_OUTER_BOUND ( 'NONE', #2267, .T. ) ;
#7775 = CARTESIAN_POINT ( 'NONE',  ( 3.535533905932738197, -31.87500000000000000, -3.535533905932738197 ) ) ;
#7776 = CARTESIAN_POINT ( 'NONE',  ( -91.33974596215551855, -10.00000000000002487, 7.500000000000001776 ) ) ;
#7777 = DIRECTION ( 'NONE',  ( 0.000000000000000000, 0.000000000000000000, -1.000000000000000000 ) ) ;
#7778 = CARTESIAN_POINT ( 'NONE',  ( -5.000000000000000000, -22.62500000273118772, -6.123233995736766282E-16 ) ) ;
#7779 = CARTESIAN_POINT ( 'NONE',  ( -0.5711823568785977523, -5.381735091635034607, -3.312500000000001776 ) ) ;
#7780 = CARTESIAN_POINT ( 'NONE',  ( -4.458734124999999437, -26.00000000136559564, -1.846868145590735644 ) ) ;
#7781 = EDGE_CURVE ( 'NONE', #6661, #10619, #6023, .T. ) ;
#7782 = DIRECTION ( 'NONE',  ( 0.000000000000000000, 0.000000000000000000, 1.000000000000000000 ) ) ;
#7783 = ORIENTED_EDGE ( 'NONE', *, *, #9727, .T. ) ;
#7784 = EDGE_LOOP ( 'NONE', ( #12511, #8904, #14499, #3007 ) ) ;
#7785 = ORIENTED_EDGE ( 'NONE', *, *, #1975, .F. ) ;
#7786 = CARTESIAN_POINT ( 'NONE',  ( -44.29799420005891619, -3.661800705855200899, 20.50793615625904209 ) ) ;
#7787 = VERTEX_POINT ( 'NONE', #14355 ) ;
#7788 = DIRECTION ( 'NONE',  ( 0.000000000000000000, 0.000000000000000000, 1.000000000000000000 ) ) ;
#7789 = CARTESIAN_POINT ( 'NONE',  ( 1.846868145590736310, -29.87500000136559564, 4.458734124999999437 ) ) ;
#7790 = CARTESIAN_POINT ( 'NONE',  ( 4.795541693661363958, 1.415196051561583790, -6.000000000000001776 ) ) ;
#7791 = CONTEXT_DEPENDENT_SHAPE_REPRESENTATION ( #13818, #7965 ) ;
#7792 = CARTESIAN_POINT ( 'NONE',  ( 0.5093500532425063732, 4.799145180956616130, -4.374999998634405252 ) ) ;
#7793 = CARTESIAN_POINT ( 'NONE',  ( 4.197393957002303999, 7.772902908466098641E-14, -3.503767560748929810 ) ) ;
#7794 = EDGE_CURVE ( 'NONE', #4537, #15165, #4094, .T. ) ;
#7796 = EDGE_CURVE ( 'NONE', #12412, #580, #4604, .T. ) ;
#7795 = VERTEX_POINT ( 'NONE', #2372 ) ;
#7797 = SURFACE_STYLE_FILL_AREA ( #12616 ) ;
#7798 = EDGE_LOOP ( 'NONE', ( #14156, #529, #308, #3677 ) ) ;
#7799 = DIRECTION ( 'NONE',  ( 0.000000000000000000, 0.000000000000000000, -1.000000000000000000 ) ) ;
#7800 = CARTESIAN_POINT ( 'NONE',  ( -4.458734125000001214, -30.87500000136559564, 1.846868145590734089 ) ) ;
#7801 = ORIENTED_EDGE ( 'NONE', *, *, #10465, .F. ) ;
#7802 = CARTESIAN_POINT ( 'NONE',  ( -2.131511515620587272, -3.916244202832140253, -7.937499998634408804 ) ) ;
#7803 = B_SPLINE_CURVE_WITH_KNOTS ( 'NONE', 3,
 ( #5246, #6542, #14867, #11306, #1283, #3790, #5087, #11142, #4024, #10100 ),
 .UNSPECIFIED., .F., .F.,
 ( 4, 2, 2, 2, 4 ),
 ( 0.000000000000000000, 0.002305503304226490767, 0.004611006608452981534, 0.006916509912679473168, 0.009222013216905964803 ),
 .UNSPECIFIED. ) ;
#7804 = CARTESIAN_POINT ( 'NONE',  ( -4.999999999999844569, 1.272547481429019856, -4.461597479913466557 ) ) ;
#7805 = AXIS2_PLACEMENT_3D ( 'NONE', #10865, #8461, #7082 ) ;
#7806 = CARTESIAN_POINT ( 'NONE',  ( 4.999999999999848121, -1.272547481429015859, -4.961597479913466557 ) ) ;
#7807 = CARTESIAN_POINT ( 'NONE',  ( 2.071067811865476394, -28.18750000000000355, 5.000000000000000000 ) ) ;
#7808 = CARTESIAN_POINT ( 'NONE',  ( -4.391654775818395251, 2.390265326283148806, -3.499999997268816276 ) ) ;
#7809 = EDGE_CURVE ( 'NONE', #1506, #3269, #14507, .T. ) ;
#7810 = PRESENTATION_STYLE_ASSIGNMENT (( #9333 ) ) ;
#7811 = CARTESIAN_POINT ( 'NONE',  ( -4.458734124999999437, -22.18750000136559564, -5.460374474430324690E-16 ) ) ;
#7812 = EDGE_CURVE ( 'NONE', #3489, #11826, #13431, .T. ) ;
#7813 = EDGE_LOOP ( 'NONE', ( #7257, #8056, #12604, #11023, #13342 ) ) ;
#7814 = CYLINDRICAL_SURFACE ( 'NONE', #5881, 6.000000000000000888 ) ;
#7815 = CARTESIAN_POINT ( 'NONE',  ( 3.033343224707661712, -3.753672977998669946, -7.499999998634409692 ) ) ;
#7816 = CARTESIAN_POINT ( 'NONE',  ( 57.73502691896258199, -4.999999999999997335, 2.081668171172168513E-14 ) ) ;
#7817 = ORIENTED_EDGE ( 'NONE', *, *, #11164, .F. ) ;
#7818 = DIRECTION ( 'NONE',  ( 0.000000000000000000, 0.000000000000000000, 1.000000000000000000 ) ) ;
#7819 = ORIENTED_EDGE ( 'NONE', *, *, #3701, .F. ) ;
#7820 = ORIENTED_EDGE ( 'NONE', *, *, #13990, .F. ) ;
#7821 = LINE ( 'NONE', #2869, #11538 ) ;
#7822 = FACE_BOUND ( 'NONE', #14814, .T. ) ;
#7823 = FACE_OUTER_BOUND ( 'NONE', #4737, .T. ) ;
#7824 = DIRECTION ( 'NONE',  ( 1.000000000000000000, 0.000000000000000000, 0.000000000000000000 ) ) ;
#7825 = CARTESIAN_POINT ( 'NONE',  ( 5.000000000000004441, -2.247904837838113790E-16, -7.920263044861759028 ) ) ;
#7826 = CARTESIAN_POINT ( 'NONE',  ( 0.000000000000000000, -13.00000000000000178, 0.000000000000000000 ) ) ;
#7827 = VECTOR ( 'NONE', #5434, 1000.000000000000000 ) ;
#7828 = CARTESIAN_POINT ( 'NONE',  ( -1.415196051561583790, 4.795541693661363958, -5.750000000000001776 ) ) ;
#7829 = CARTESIAN_POINT ( 'NONE',  ( 3.061616997868383141E-16, -29.75000000000000000, -5.000000000000000000 ) ) ;
#7830 = AXIS2_PLACEMENT_3D ( 'NONE', #13043, #7008, #6767 ) ;
#7831 = FACE_OUTER_BOUND ( 'NONE', #11358, .T. ) ;
#7832 = CYLINDRICAL_SURFACE ( 'NONE', #15374, 5.000000000000000000 ) ;
#7833 = ADVANCED_FACE ( 'NONE', ( #10719 ), #7168, .F. ) ;
#7834 = CARTESIAN_POINT ( 'NONE',  ( -1.261996585732579224, 4.276409079477648589, -6.312499998634407028 ) ) ;
#7835 = VERTEX_POINT ( 'NONE', #7083 ) ;
#7836 = CARTESIAN_POINT ( 'NONE',  ( 2.602085213965210642E-15, 8.660254037844392627, -7.422398894150035176 ) ) ;
#7837 = VERTEX_POINT ( 'NONE', #12220 ) ;
#7838 = ORIENTED_EDGE ( 'NONE', *, *, #11222, .F. ) ;
#7839 = VERTEX_POINT ( 'NONE', #3595 ) ;
#7840 = CARTESIAN_POINT ( 'NONE',  ( -4.458734124999999437, -29.18750000136559564, -5.460374474430324690E-16 ) ) ;
#7841 = CYLINDRICAL_SURFACE ( 'NONE', #6888, 2.500000000000909495 ) ;
#7842 = EDGE_LOOP ( 'NONE', ( #1714, #4918 ) ) ;
#7843 = FACE_OUTER_BOUND ( 'NONE', #11219, .T. ) ;
#7844 = DIRECTION ( 'NONE',  ( 0.000000000000000000, -0.4999999999999993894, 0.8660254037844389297 ) ) ;
#7845 = DIRECTION ( 'NONE',  ( 0.000000000000000000, 0.5000000000000012212, 0.8660254037844380415 ) ) ;
#7846 = CARTESIAN_POINT ( 'NONE',  ( -2.071067811865475061, -29.68750000000000711, -5.000000000000000888 ) ) ;
#7847 = CARTESIAN_POINT ( 'NONE',  ( 0.5093500532425063732, 4.799145180956616130, -5.124999998634405252 ) ) ;
#7848 = CARTESIAN_POINT ( 'NONE',  ( -4.336808689942017736E-16, -8.660254037844399733, -7.422398894150038728 ) ) ;
#7849 = DIRECTION ( 'NONE',  ( -0.000000000000000000, -0.000000000000000000, -1.000000000000000000 ) ) ;
#7850 = CARTESIAN_POINT ( 'NONE',  ( -5.000000000000000888, -25.68750000273119127, -2.071067811865475949 ) ) ;
#7851 = ADVANCED_FACE ( 'NONE', ( #4809 ), #858, .T. ) ;
#7852 = DIRECTION ( 'NONE',  ( 0.000000000000000000, 0.000000000000000000, 1.000000000000000000 ) ) ;
#7853 = CARTESIAN_POINT ( 'NONE',  ( 1.846868145590736310, -26.62500000136559564, 4.458734124999997661 ) ) ;
#7854 = DIRECTION ( 'NONE',  ( 0.000000000000000000, 1.000000000000000000, 0.000000000000000000 ) ) ;
#7855 = ORIENTED_EDGE ( 'NONE', *, *, #15532, .T. ) ;
#7856 = ORIENTED_EDGE ( 'NONE', *, *, #2867, .F. ) ;
#7857 = VERTEX_POINT ( 'NONE', #11985 ) ;
#7858 = CARTESIAN_POINT ( 'NONE',  ( 4.154306624731035846, -2.398490048085128556, -3.721999068284417955 ) ) ;
#7859 = ORIENTED_EDGE ( 'NONE', *, *, #4019, .T. ) ;
#7860 = DIRECTION ( 'NONE',  ( -1.000000000000000000, 0.000000000000000000, -0.000000000000000000 ) ) ;
#7861 = EDGE_CURVE ( 'NONE', #12016, #4219, #5865, .T. ) ;
#7862 = EDGE_CURVE ( 'NONE', #4061, #10685, #1084, .T. ) ;
#7863 = CARTESIAN_POINT ( 'NONE',  ( -3.535533905932738641, -31.37500000000000000, 3.535533905932737309 ) ) ;
#7864 = CARTESIAN_POINT ( 'NONE',  ( 4.458734124999999437, -29.75000000136559564, 1.846868145590737864 ) ) ;
#7865 =( GEOMETRIC_REPRESENTATION_CONTEXT ( 3 ) GLOBAL_UNCERTAINTY_ASSIGNED_CONTEXT ( ( #7883 ) ) GLOBAL_UNIT_ASSIGNED_CONTEXT ( ( #10114, #8080, #12975 ) ) REPRESENTATION_CONTEXT ( 'NONE', 'WORKASPACE' ) );
#7866 = CARTESIAN_POINT ( 'NONE',  ( 4.209348295687701302, 3.401574460001766109, -0.8124999972688135008 ) ) ;
#7867 = SHAPE_DEFINITION_REPRESENTATION ( #10928, #7495 ) ;
#7868 = CARTESIAN_POINT ( 'NONE',  ( -3.033343224707664376, 3.753672977998667726, -8.249999998634409692 ) ) ;
#7869 = VERTEX_POINT ( 'NONE', #13127 ) ;
#7870 =( NAMED_UNIT ( * ) PLANE_ANGLE_UNIT ( ) SI_UNIT ( $, .RADIAN. ) );
#7871 = ORIENTED_EDGE ( 'NONE', *, *, #1378, .T. ) ;
#7872 = CARTESIAN_POINT ( 'NONE',  ( -115.0000000000000000, -10.00000000000000888, -7.500000000000000000 ) ) ;
#7873 = CARTESIAN_POINT ( 'NONE',  ( -8.190561711645485556E-16, -27.68750000136559564, 4.458734124999999437 ) ) ;
#7874 = AXIS2_PLACEMENT_3D ( 'NONE', #4550, #10696, #8523 ) ;
#7875 = VERTEX_POINT ( 'NONE', #3503 ) ;
#7876 = CIRCLE ( 'NONE', #8916, 5.000000000000001776 ) ;
#7877 = CARTESIAN_POINT ( 'NONE',  ( -3.401574460001765221, 4.209348295687701302, -4.687500000000000888 ) ) ;
#7878 = EDGE_CURVE ( 'NONE', #7055, #10036, #14940, .T. ) ;
#7879 = EDGE_CURVE ( 'NONE', #13350, #14899, #4650, .T. ) ;
#7880 = LINE ( 'NONE', #10062, #4371 ) ;
#7881 = CARTESIAN_POINT ( 'NONE',  ( -5.000000000000092371, -0.7223674278660636716, -8.396799362785968057 ) ) ;
#7882 = STYLED_ITEM ( 'NONE', ( #5851 ), #9085 ) ;
#7883 = UNCERTAINTY_MEASURE_WITH_UNIT (LENGTH_MEASURE( 1.000000000000000082E-05 ), #10114, 'distance_accuracy_value', 'NONE');
#7884 = AXIS2_PLACEMENT_3D ( 'NONE', #2192, #11962, #5837 ) ;
#7885 = CARTESIAN_POINT ( 'NONE',  ( 4.209348295687701302, 3.401574460001765665, -7.812499997268815832 ) ) ;
#7886 = DIRECTION ( 'NONE',  ( -0.000000000000000000, 1.000000000000000000, -0.000000000000000000 ) ) ;
#7887 = FACE_OUTER_BOUND ( 'NONE', #6202, .T. ) ;
#7888 = ORIENTED_EDGE ( 'NONE', *, *, #6286, .T. ) ;
#7889 = CIRCLE ( 'NONE', #14071, 2.000000000000000888 ) ;
#7890 = DIRECTION ( 'NONE',  ( 1.000000000000000000, 0.000000000000000000, 0.000000000000000000 ) ) ;
#7891 = LINE ( 'NONE', #4155, #12022 ) ;
#7892 = DIRECTION ( 'NONE',  ( -0.000000000000000000, -0.000000000000000000, 1.000000000000000000 ) ) ;
#7893 = ORIENTED_EDGE ( 'NONE', *, *, #10447, .T. ) ;
#7894 = DIRECTION ( 'NONE',  ( -0.000000000000000000, -0.000000000000000000, -1.000000000000000000 ) ) ;
#7895 = ORIENTED_EDGE ( 'NONE', *, *, #4216, .T. ) ;
#7896 = VERTEX_POINT ( 'NONE', #15888 ) ;
#7897 = CARTESIAN_POINT ( 'NONE',  ( 19.99999999999956657, -8.786575603324269439E-13, -11.50000000000000000 ) ) ;
#7898 = CARTESIAN_POINT ( 'NONE',  ( 0.000000000000000000, -20.00000000000000000, 0.000000000000000000 ) ) ;
#7899 = CIRCLE ( 'NONE', #6083, 2.649999999999992806 ) ;
#7900 = PLANE ( 'NONE',  #9418 ) ;
#7901 = ADVANCED_FACE ( 'NONE', ( #9733, #8462 ), #13360, .F. ) ;
#7902 = AXIS2_PLACEMENT_3D ( 'NONE', #7441, #4683, #8650 ) ;
#7903 = DIRECTION ( 'NONE',  ( -1.000000000000000000, -0.000000000000000000, -0.000000000000000000 ) ) ;
#7904 = FACE_OUTER_BOUND ( 'NONE', #773, .T. ) ;
#7905 = DIRECTION ( 'NONE',  ( -0.000000000000000000, 1.000000000000000000, -0.000000000000000000 ) ) ;
#7906 = CARTESIAN_POINT ( 'NONE',  ( 0.000000000000000000, 0.000000000000000000, -4.000000000000000000 ) ) ;
#7907 = CARTESIAN_POINT ( 'NONE',  ( 2.071067811865447528, -24.93750000273118417, -5.000000000000029310 ) ) ;
#7908 = CARTESIAN_POINT ( 'NONE',  ( 4.458734124999999437, -24.50000000136559564, 1.846868145590737864 ) ) ;
#7909 = CARTESIAN_POINT ( 'NONE',  ( 3.753672977998667726, 3.033343224707664376, -5.499999998634407916 ) ) ;
#7910 = EDGE_LOOP ( 'NONE', ( #2022, #12076 ) ) ;
#7911 = VECTOR ( 'NONE', #15402, 1000.000000000000000 ) ;
#7912 = LINE ( 'NONE', #5234, #1441 ) ;
#7913 = ORIENTED_EDGE ( 'NONE', *, *, #9991, .T. ) ;
#7914 = VERTEX_POINT ( 'NONE', #1494 ) ;
#7915 = AXIS2_PLACEMENT_3D ( 'NONE', #1027, #15823, #9660 ) ;
#7916 = CARTESIAN_POINT ( 'NONE',  ( 3.152801135295366208, -30.81250000136559564, 3.152801135295367985 ) ) ;
#7917 = FACE_OUTER_BOUND ( 'NONE', #4864, .T. ) ;
#7918 = ORIENTED_EDGE ( 'NONE', *, *, #1483, .T. ) ;
#7919 = CARTESIAN_POINT ( 'NONE',  ( -5.000000000000000888, 6.123233995736767268E-16, -25.03750572909317285 ) ) ;
#7920 = EDGE_CURVE ( 'NONE', #15685, #7141, #10137, .T. ) ;
#7921 = CIRCLE ( 'NONE', #15449, 2.499999999999998668 ) ;
#7922 = ADVANCED_FACE ( 'NONE', ( #7649, #3907 ), #7735, .T. ) ;
#7923 =( BOUNDED_SURFACE ( )  B_SPLINE_SURFACE ( 3, 2, ( 
 ( #8892, #8008, #1767 ),
 ( #10505, #12739, #801 ),
 ( #12905, #725, #12823 ),
 ( #9366, #15516, #15352 ),
 ( #15438, #4271, #4361 ),
 ( #2971, #14290, #13961 ),
 ( #11539, #1685, #5412 ),
 ( #489, #3139, #14046 ) ),
 .UNSPECIFIED., .F., .F., .F. ) 
 B_SPLINE_SURFACE_WITH_KNOTS ( ( 4, 2, 2, 4 ),
 ( 3, 3 ),
 ( 0.03850042371095789562, 0.04313406099830586343, 0.04545087964197984387, 0.04776769828565383125 ),
 ( 0.000000000000000000, 1.000000000000000000 ),
 .UNSPECIFIED. ) 
 GEOMETRIC_REPRESENTATION_ITEM ( )  RATIONAL_B_SPLINE_SURFACE ( (
 ( 1.000000000000000000, 0.8047781847388131293, 1.000000000000000000),
 ( 1.000000000000000000, 0.8123760230792201886, 1.000000000000000000),
 ( 1.000000000000000000, 0.8190653851697322629, 1.000000000000000000),
 ( 1.000000000000000000, 0.8191940386278004915, 1.000000000000000000),
 ( 1.000000000000000000, 0.8176096570058365431, 1.000000000000000000),
 ( 1.000000000000000000, 0.8122964723274869181, 1.000000000000000000),
 ( 1.000000000000000000, 0.8086312464134836064, 1.000000000000000000),
 ( 1.000000000000000000, 0.8047712192439642198, 1.000000000000000000) ) ) 
 REPRESENTATION_ITEM ( '' )  SURFACE ( )  );
#7924 = CIRCLE ( 'NONE', #14843, 39.99999999999999289 ) ;
#7925 = LINE ( 'NONE', #3215, #12866 ) ;
#7926 = CARTESIAN_POINT ( 'NONE',  ( 3.753672977998667726, 3.033343224707664820, -7.249999998634409692 ) ) ;
#7927 = CARTESIAN_POINT ( 'NONE',  ( -21.01110699893041911, -3.000000000000001332, -36.39230484541334221 ) ) ;
#7928 = AXIS2_PLACEMENT_3D ( 'NONE', #12401, #11435, #310 ) ;
#7929 = CARTESIAN_POINT ( 'NONE',  ( -3.535533905932738641, -25.37500000000000000, 3.535533905932737309 ) ) ;
#7930 = CIRCLE ( 'NONE', #1461, 31.99999999999999289 ) ;
#7931 = CARTESIAN_POINT ( 'NONE',  ( 2.131511515620586383, 3.916244202832140253, -4.187499998634405252 ) ) ;
#7932 = DIRECTION ( 'NONE',  ( -1.000000000000000000, 0.000000000000000000, 0.000000000000000000 ) ) ;
#7933 = DIRECTION ( 'NONE',  ( 0.000000000000000000, 0.000000000000000000, 1.000000000000000000 ) ) ;
#7934 = CARTESIAN_POINT ( 'NONE',  ( -3.535533905932737309, -22.75000000273118772, -3.535533905932738197 ) ) ;
#7935 = CARTESIAN_POINT ( 'NONE',  ( -45.00000000000000000, 0.000000000000000000, 7.500000000000001776 ) ) ;
#7936 = CARTESIAN_POINT ( 'NONE',  ( -1.846868145590737420, -26.75000000136559564, 4.458734124999997661 ) ) ;
#7937 = FACE_BOUND ( 'NONE', #5849, .T. ) ;
#7938 = VERTEX_POINT ( 'NONE', #14826 ) ;
#7939 = VECTOR ( 'NONE', #5547, 1000.000000000000114 ) ;
#7940 = ORIENTED_EDGE ( 'NONE', *, *, #6221, .T. ) ;
#7941 = DIRECTION ( 'NONE',  ( 9.912705577010324563E-16, 0.000000000000000000, 1.000000000000000000 ) ) ;
#7942 = PRODUCT_DEFINITION_SHAPE ( 'NONE', 'NONE',  #15986 ) ;
#7943 = VERTEX_POINT ( 'NONE', #9816 ) ;
#7944 = CARTESIAN_POINT ( 'NONE',  ( 4.391654775818395251, -2.390265326283149694, -6.999999997268815832 ) ) ;
#7945 = VERTEX_POINT ( 'NONE', #8853 ) ;
#7946 = CARTESIAN_POINT ( 'NONE',  ( 5.809475019311125976, -13.00000000000000178, -1.500000000000000000 ) ) ;
#7947 = EDGE_CURVE ( 'NONE', #6071, #15584, #9514, .T. ) ;
#7948 = DIRECTION ( 'NONE',  ( 0.8660254037844387076, 0.000000000000000000, -0.4999999999999998890 ) ) ;
#7949 = CARTESIAN_POINT ( 'NONE',  ( -4.458734124999999437, -26.18750000136559919, -5.460374474430324690E-16 ) ) ;
#7950 = CARTESIAN_POINT ( 'NONE',  ( -3.401574460001765221, 4.209348295687701302, -0.5624999972688168315 ) ) ;
#7951 = CARTESIAN_POINT ( 'NONE',  ( 4.276409079477644148, 1.261996585732577891, -8.562499998634409692 ) ) ;
#7952 = FACE_OUTER_BOUND ( 'NONE', #13496, .T. ) ;
#7953 = ORIENTED_EDGE ( 'NONE', *, *, #12927, .T. ) ;
#7954 =( NAMED_UNIT ( * ) SI_UNIT ( $, .STERADIAN. ) SOLID_ANGLE_UNIT ( ) );
#7955 = CIRCLE ( 'NONE', #15733, 6.000000000000000888 ) ;
#7956 = ORIENTED_EDGE ( 'NONE', *, *, #13326, .F. ) ;
#7957 = LINE ( 'NONE', #9010, #8738 ) ;
#7958 = CARTESIAN_POINT ( 'NONE',  ( -8.190561711645485556E-16, -29.68750000136559208, 4.458734124999999437 ) ) ;
#7959 = ORIENTED_EDGE ( 'NONE', *, *, #1161, .F. ) ;
#7960 = CIRCLE ( 'NONE', #14924, 2.649999999999999467 ) ;
#7961 = LINE ( 'NONE', #4468, #8160 ) ;
#7962 = CARTESIAN_POINT ( 'NONE',  ( -1.154700538379222596, 0.000000000000000000, -34.00000000000000000 ) ) ;
#7963 = DIRECTION ( 'NONE',  ( -0.000000000000000000, -0.000000000000000000, -1.000000000000000000 ) ) ;
#7964 = COLOUR_RGB ( '', 0.09019608, 0.27058824, 0.51372549) ;
#7965 = PRODUCT_DEFINITION_SHAPE ( 'NONE', 'NONE',  #15975 ) ;
#7966 = CARTESIAN_POINT ( 'NONE',  ( -4.209348295687703967, -3.401574460001763001, -8.312499997268812280 ) ) ;
#7967 = CARTESIAN_POINT ( 'NONE',  ( 47.32050807568875683, -37.00000000000000711, 41.96152422706633445 ) ) ;
#7968 = FILL_AREA_STYLE_COLOUR ( '', #12065 ) ;
#7969 = CARTESIAN_POINT ( 'NONE',  ( 3.061616997868383141E-16, -28.75000000000000000, -5.000000000000000000 ) ) ;
#7970 = EDGE_LOOP ( 'NONE', ( #8991, #3913, #4714, #1702 ) ) ;
#7971 = CARTESIAN_POINT ( 'NONE',  ( 7.499999999999999112, 1.854554393013824631, -0.1880126015361718583 ) ) ;
#7972 = CARTESIAN_POINT ( 'NONE',  ( -55.00000000000000000, 0.000000000000000000, 19.99999999999999289 ) ) ;
#7973 = VECTOR ( 'NONE', #7073, 1000.000000000000000 ) ;
#7974 = CARTESIAN_POINT ( 'NONE',  ( 3.750000000000005773, 6.495190528383288253, 0.000000000000000000 ) ) ;
#7975 = ADVANCED_FACE ( 'NONE', ( #12305 ), #1568, .T. ) ;
#7976 = ORIENTED_EDGE ( 'NONE', *, *, #8376, .T. ) ;
#7977 = PLANE ( 'NONE',  #7220 ) ;
#7978 = ORIENTED_EDGE ( 'NONE', *, *, #10842, .F. ) ;
#7979 = ORIENTED_EDGE ( 'NONE', *, *, #14351, .F. ) ;
#7980 = CYLINDRICAL_SURFACE ( 'NONE', #9383, 2.000000000000000888 ) ;
#7981 = PLANE ( 'NONE',  #7412 ) ;
#7982 = VECTOR ( 'NONE', #7564, 1000.000000000000114 ) ;
#7983 = VECTOR ( 'NONE', #2398, 1000.000000000000000 ) ;
#7984 = DIRECTION ( 'NONE',  ( 0.000000000000000000, -0.000000000000000000, 1.000000000000000000 ) ) ;
#7985 = AXIS2_PLACEMENT_3D ( 'NONE', #10869, #8464, #7403 ) ;
#7986 = CIRCLE ( 'NONE', #1512, 6.000000000000000888 ) ;
#7987 = DIRECTION ( 'NONE',  ( -0.000000000000000000, 1.000000000000000000, -0.000000000000000000 ) ) ;
#7988 = DIRECTION ( 'NONE',  ( 0.000000000000000000, 1.000000000000000000, 0.000000000000000000 ) ) ;
#7989 = PLANE ( 'NONE',  #12347 ) ;
#7990 = DIRECTION ( 'NONE',  ( 0.000000000000000000, 1.000000000000000000, 0.000000000000000000 ) ) ;
#7991 = CARTESIAN_POINT ( 'NONE',  ( 31.75426480542940766, -37.00000000000000711, 15.00000000000001243 ) ) ;
#7992 = CIRCLE ( 'NONE', #4619, 2.000000000000000888 ) ;
#7993 = CARTESIAN_POINT ( 'NONE',  ( -44.43375672972994295, 0.000000000000000000, -19.99999999999594635 ) ) ;
#7994 = CARTESIAN_POINT ( 'NONE',  ( 2.730187237215162345E-16, -24.18750000136559564, -4.458734124999999437 ) ) ;
#7995 = AXIS2_PLACEMENT_3D ( 'NONE', #9767, #13541, #13457 ) ;
#7996 = CARTESIAN_POINT ( 'NONE',  ( 3.033343224707661712, -3.753672977998669946, -6.749999998634408804 ) ) ;
#7997 = VERTEX_POINT ( 'NONE', #10066 ) ;
#7998 = CARTESIAN_POINT ( 'NONE',  ( -2.666517441655246264E-14, 8.895721644649745130, -7.917989418073288377 ) ) ;
#7999 = EDGE_CURVE ( 'NONE', #15267, #8315, #7391, .T. ) ;
#8000 = ORIENTED_EDGE ( 'NONE', *, *, #11671, .F. ) ;
#8001 = VERTEX_POINT ( 'NONE', #12547 ) ;
#8002 = EDGE_CURVE ( 'NONE', #15369, #8388, #1321, .T. ) ;
#8003 = SURFACE_STYLE_FILL_AREA ( #15511 ) ;
#8004 = CARTESIAN_POINT ( 'NONE',  ( 2.730187237215162345E-16, -29.43750000136559208, -4.458734124999999437 ) ) ;
#8005 = LINE ( 'NONE', #11688, #6098 ) ;
#8006 = ORIENTED_EDGE ( 'NONE', *, *, #11241, .T. ) ;
#8007 = DIRECTION ( 'NONE',  ( 0.000000000000000000, 1.000000000000000000, 0.000000000000000000 ) ) ;
#8008 = CARTESIAN_POINT ( 'NONE',  ( 7.500000000000000888, -4.651016565836978423, -7.928861822685568050 ) ) ;
#8009 = CARTESIAN_POINT ( 'NONE',  ( 3.753672977998667726, 3.033343224707664820, -5.249999998634407916 ) ) ;
#8010 = CARTESIAN_POINT ( 'NONE',  ( 0.5984201754795555050, 8.314755988442760426, -0.7022220667781343684 ) ) ;
#8011 = B_SPLINE_CURVE_WITH_KNOTS ( 'NONE', 3,
 ( #6548, #15109, #4029, #8980, #13892, #11463, #5335, #12828 ),
 .UNSPECIFIED., .F., .F.,
 ( 4, 2, 2, 4 ),
 ( 0.000000000000000000, 0.002450665683189820997, 0.003675998524784731495, 0.004901331366379641993 ),
 .UNSPECIFIED. ) ;
#8012 = CARTESIAN_POINT ( 'NONE',  ( 3.061616997868383141E-16, -24.75000000000000000, -5.000000000000000000 ) ) ;
#8013 = CARTESIAN_POINT ( 'NONE',  ( -0.5093500532425060401, -4.799145180956616130, -6.624999998634407916 ) ) ;
#8014 = CARTESIAN_POINT ( 'NONE',  ( 0.000000000000000000, 0.000000000000000000, -25.03750572909317285 ) ) ;
#8015 = DIRECTION ( 'NONE',  ( -1.000000000000000000, 0.000000000000000000, 0.000000000000000000 ) ) ;
#8016 = CARTESIAN_POINT ( 'NONE',  ( 3.535533905932736864, -24.25000000273118772, 3.535533905932738641 ) ) ;
#8017 = VERTEX_POINT ( 'NONE', #3982 ) ;
#8018 = CARTESIAN_POINT ( 'NONE',  ( 1.846868145590736310, -25.62500000136559564, 4.458734124999997661 ) ) ;
#8019 = EDGE_CURVE ( 'NONE', #6755, #3455, #13447, .T. ) ;
#8020 = CARTESIAN_POINT ( 'NONE',  ( -0.04606493828583544531, -9.175055303659563677, -8.057411785091796119 ) ) ;
#8021 = ORIENTED_EDGE ( 'NONE', *, *, #223, .T. ) ;
#8022 = ORIENTED_EDGE ( 'NONE', *, *, #4689, .F. ) ;
#8023 = ADVANCED_FACE ( 'NONE', ( #11345 ), #6191, .T. ) ;
#8024 = CARTESIAN_POINT ( 'NONE',  ( 2.390265326283148806, 4.391654775818395251, -3.749999997268816720 ) ) ;
#8025 = AXIS2_PLACEMENT_3D ( 'NONE', #11891, #8293, #3020 ) ;
#8026 = VERTEX_POINT ( 'NONE', #11266 ) ;
#8027 = LINE ( 'NONE', #10751, #10479 ) ;
#8028 =( BOUNDED_CURVE ( )  B_SPLINE_CURVE ( 2, ( #5782, #11035, #2305, #13364, #4729, #9735, #4653, #13510, #7250 ),
 .UNSPECIFIED., .F., .F. ) 
 B_SPLINE_CURVE_WITH_KNOTS ( ( 3, 2, 2, 2, 3 ),
 ( 0.8250000000000000666, 0.8375000000000001332, 0.8500000000000000888, 0.8625000000000000444, 0.8750000000000000000 ),
 .UNSPECIFIED. ) 
 CURVE ( )  GEOMETRIC_REPRESENTATION_ITEM ( )  RATIONAL_B_SPLINE_CURVE ( ( 0.9999999999999993339, 0.9238795325112874046, 1.000000000000000000, 0.9238795325112867385, 1.000000000000000000, 0.9238795325112867385, 1.000000000000000000, 0.9238795325112867385, 1.000000000000000000 ) ) 
 REPRESENTATION_ITEM ( '' )  );
#8029 = VERTEX_POINT ( 'NONE', #214 ) ;
#8030 = CARTESIAN_POINT ( 'NONE',  ( 42.02221399786069611, -3.000000000000000000, -2.649999999999888445 ) ) ;
#8031 = CARTESIAN_POINT ( 'NONE',  ( -90.00000000000000000, -95.00000000000000000, 7.500000000000001776 ) ) ;
#8032 = CARTESIAN_POINT ( 'NONE',  ( -1.846868145590737420, -27.00000000136559208, 4.458734124999999437 ) ) ;
#8033 = CARTESIAN_POINT ( 'NONE',  ( 4.209348295687701302, 3.401574460001766109, -6.812499997268814944 ) ) ;
#8034 = CARTESIAN_POINT ( 'NONE',  ( -4.209348295687703079, -3.401574460001763445, -4.437500000000001776 ) ) ;
#8035 = SHAPE_DEFINITION_REPRESENTATION ( #7067, #3049 ) ;
#8036 = CYLINDRICAL_SURFACE ( 'NONE', #2001, 5.000000000000000888 ) ;
#8037 = CARTESIAN_POINT ( 'NONE',  ( -28.86751345948129099, 1.999999999999998224, 18.00000000000000000 ) ) ;
#8038 = ADVANCED_FACE ( 'NONE', ( #47 ), #3746, .T. ) ;
#8039 = ORIENTED_EDGE ( 'NONE', *, *, #250, .F. ) ;
#8040 = EDGE_CURVE ( 'NONE', #509, #3920, #11714, .T. ) ;
#8041 = EDGE_LOOP ( 'NONE', ( #9436, #10937, #4079, #8572, #9497 ) ) ;
#8042 = DIRECTION ( 'NONE',  ( 0.000000000000000000, -1.000000000000000000, 0.000000000000000000 ) ) ;
#8043 = ORIENTED_EDGE ( 'NONE', *, *, #7519, .F. ) ;
#8044 = DIRECTION ( 'NONE',  ( 1.000000000000000000, 0.000000000000000000, 0.000000000000000000 ) ) ;
#8045 = DIRECTION ( 'NONE',  ( 0.000000000000000000, 1.000000000000000000, 0.000000000000000000 ) ) ;
#8046 = CARTESIAN_POINT ( 'NONE',  ( 0.6507732100473444525, -4.243078065514795050, -0.2236248678334952777 ) ) ;
#8047 = CARTESIAN_POINT ( 'NONE',  ( 2.390265326283148806, 4.391654775818395251, -6.749999997268815832 ) ) ;
#8048 = CARTESIAN_POINT ( 'NONE',  ( 7.347880794884118356E-15, 37.00000000000000000, 60.00000000000000000 ) ) ;
#8049 = CARTESIAN_POINT ( 'NONE',  ( 0.5711823568785988625, 5.381735091635026613, -1.812500000000000666 ) ) ;
#8050 = DIRECTION ( 'NONE',  ( 0.000000000000000000, -0.000000000000000000, -1.000000000000000000 ) ) ;
#8051 = EDGE_LOOP ( 'NONE', ( #12733, #6794, #8678, #7455 ) ) ;
#8052 = CARTESIAN_POINT ( 'NONE',  ( -67.50000000000000000, 40.00000000000000000, -7.070249711157346244E-13 ) ) ;
#8053 = DIRECTION ( 'NONE',  ( -0.8660254037844405950, 0.4999999999999965028, 0.000000000000000000 ) ) ;
#8054 = EDGE_CURVE ( 'NONE', #14880, #9569, #11640, .T. ) ;
#8055 = LINE ( 'NONE', #11738, #5328 ) ;
#8056 = ORIENTED_EDGE ( 'NONE', *, *, #5540, .T. ) ;
#8057 = CARTESIAN_POINT ( 'NONE',  ( 42.02221399786069611, -3.000000000000001332, -2.649999999999881783 ) ) ;
#8058 = ORIENTED_EDGE ( 'NONE', *, *, #3562, .F. ) ;
#8059 = ORIENTED_EDGE ( 'NONE', *, *, #9292, .T. ) ;
#8060 = CARTESIAN_POINT ( 'NONE',  ( -36.99999999999999289, -11.00000000000000178, 2.000000000000830891 ) ) ;
#8061 = CARTESIAN_POINT ( 'NONE',  ( -1.257172072275743346, 3.892973519171203378, -3.433252694550776862 ) ) ;
#8062 = CARTESIAN_POINT ( 'NONE',  ( -7.500000000000007105, 3.639598441879744239, -0.7155132341745296110 ) ) ;
#8063 = B_SPLINE_CURVE_WITH_KNOTS ( 'NONE', 3,
 ( #8124, #4548, #8287, #15714, #13178, #9403, #13019, #11727 ),
 .UNSPECIFIED., .F., .F.,
 ( 4, 2, 2, 4 ),
 ( 2.465131517075058656E-07, 0.001183067374689851080, 0.001774477805458923299, 0.002365888236227995517 ),
 .UNSPECIFIED. ) ;
#8064 = APPLICATION_CONTEXT ( 'automotive_design' ) ;
#8065 = EDGE_CURVE ( 'NONE', #1633, #12516, #6261, .T. ) ;
#8066 = CARTESIAN_POINT ( 'NONE',  ( 0.000000000000000000, 0.000000000000000000, -4.974599999999998801 ) ) ;
#8067 = CARTESIAN_POINT ( 'NONE',  ( -5.000000000000000888, -25.56250000000000355, -2.071067811865475949 ) ) ;
#8068 = CARTESIAN_POINT ( 'NONE',  ( -9.184850993605147944E-16, -23.25000000000000000, 5.000000000000000000 ) ) ;
#8069 = DIRECTION ( 'NONE',  ( 1.000000000000000000, 0.000000000000000000, 0.000000000000000000 ) ) ;
#8070 = DIRECTION ( 'NONE',  ( 0.000000000000000000, 1.000000000000000000, 0.000000000000000000 ) ) ;
#8071 = AXIS2_PLACEMENT_3D ( 'NONE', #2029, #15613, #4533 ) ;
#8072 = CARTESIAN_POINT ( 'NONE',  ( 5.000000000000000000, -25.18750000273118772, 2.071067811865478614 ) ) ;
#8073 = CARTESIAN_POINT ( 'NONE',  ( -4.458734124999999437, -29.18750000136559564, -5.460374474430324690E-16 ) ) ;
#8074 = CARTESIAN_POINT ( 'NONE',  ( 1.261996585732578113, -4.276409079477644148, -0.5624999986344088043 ) ) ;
#8075 = EDGE_LOOP ( 'NONE', ( #4122, #13632 ) ) ;
#8076 = UNCERTAINTY_MEASURE_WITH_UNIT (LENGTH_MEASURE( 1.000000000000000082E-05 ), #8304, 'distance_accuracy_value', 'NONE');
#8077 = DIRECTION ( 'NONE',  ( 0.000000000000000000, 1.000000000000000000, 0.000000000000000000 ) ) ;
#8078 = ORIENTED_EDGE ( 'NONE', *, *, #11102, .F. ) ;
#8079 = ORIENTED_EDGE ( 'NONE', *, *, #3515, .F. ) ;
#8080 =( NAMED_UNIT ( * ) PLANE_ANGLE_UNIT ( ) SI_UNIT ( $, .RADIAN. ) );
#8081 = CARTESIAN_POINT ( 'NONE',  ( -4.458734124999999437, -25.18750000136559564, -5.460374474430324690E-16 ) ) ;
#8082 = CARTESIAN_POINT ( 'NONE',  ( 2.687328764639642653, -3.067272167851299969, -0.05923475698271395140 ) ) ;
#8083 = CYLINDRICAL_SURFACE ( 'NONE', #5322, 32.00000000000000711 ) ;
#8084 = LINE ( 'NONE', #5569, #9774 ) ;
#8085 = EDGE_CURVE ( 'NONE', #12657, #379, #11953, .T. ) ;
#8086 = AXIS2_PLACEMENT_3D ( 'NONE', #9115, #15086, #4003 ) ;
#8087 = CARTESIAN_POINT ( 'NONE',  ( 1.261996585732578113, -4.276409079477644148, -6.562499998634407028 ) ) ;
#8088 = CARTESIAN_POINT ( 'NONE',  ( -28.86751345948129455, -4.999999999999997335, 20.00000000000000355 ) ) ;
#8089 = ADVANCED_FACE ( 'NONE', ( #823 ), #4616, .F. ) ;
#8090 = CARTESIAN_POINT ( 'NONE',  ( 2.071067811865476394, -27.18750000000000355, 5.000000000000000000 ) ) ;
#8091 = CARTESIAN_POINT ( 'NONE',  ( -3.916244202832140253, 2.131511515620587272, -5.937499998634407028 ) ) ;
#8092 = FACE_OUTER_BOUND ( 'NONE', #1832, .T. ) ;
#8093 = DIRECTION ( 'NONE',  ( 0.000000000000000000, 0.000000000000000000, -1.000000000000000000 ) ) ;
#8094 = CARTESIAN_POINT ( 'NONE',  ( 5.000000000000000000, -24.18750000273119127, 2.071067811865478614 ) ) ;
#8095 = ORIENTED_EDGE ( 'NONE', *, *, #6819, .F. ) ;
#8096 = CARTESIAN_POINT ( 'NONE',  ( -8.190561711645485556E-16, -25.68750000136559564, 4.458734124999999437 ) ) ;
#8097 = CARTESIAN_POINT ( 'NONE',  ( 5.112021521198525598, -5.708827036477267747, -7.069802615102038779 ) ) ;
#8098 = ORIENTED_EDGE ( 'NONE', *, *, #7947, .F. ) ;
#8099 = ORIENTED_EDGE ( 'NONE', *, *, #2831, .F. ) ;
#8100 = CARTESIAN_POINT ( 'NONE',  ( -7.500000000000671463, 3.157052757790888453, -7.642767288269949333 ) ) ;
#8101 = AXIS2_PLACEMENT_3D ( 'NONE', #4209, #2996, #7948 ) ;
#8102 = AXIS2_PLACEMENT_3D ( 'NONE', #1605, #10102, #3949 ) ;
#8103 = CYLINDRICAL_SURFACE ( 'NONE', #5822, 1.999999999999998668 ) ;
#8104 = ORIENTED_EDGE ( 'NONE', *, *, #6577, .T. ) ;
#8105 = CARTESIAN_POINT ( 'NONE',  ( -5.560781378645575757, 6.809993116116508640E-16, -4.000000000000000000 ) ) ;
#8106 = PRODUCT_DEFINITION_SHAPE ( 'NONE', 'NONE',  #15976 ) ;
#8107 = CARTESIAN_POINT ( 'NONE',  ( -4.154094228333736538, -2.398367420967545627, -3.721909803043222276 ) ) ;
#8108 = EDGE_CURVE ( 'NONE', #5616, #1597, #7049, .T. ) ;
#8109 = CARTESIAN_POINT ( 'NONE',  ( 4.458734124999999437, -25.68750000136559564, 0.000000000000000000 ) ) ;
#8110 = CARTESIAN_POINT ( 'NONE',  ( 0.6810597143197052450, 4.461075778259290914, -3.598441714920602053 ) ) ;
#8111 = CARTESIAN_POINT ( 'NONE',  ( 4.729367062499999719, -31.84375000068279959, 0.000000000000000000 ) ) ;
#8112 = ITEM_DEFINED_TRANSFORMATION ( 'NONE', 'NONE', #6054,  #3223 ) ;
#8113 = DIRECTION ( 'NONE',  ( 0.000000000000000000, 0.000000000000000000, 1.000000000000000000 ) ) ;
#8114 = EDGE_LOOP ( 'NONE', ( #8789, #1542, #2184, #10939, #9742, #1869, #8754 ) ) ;
#8115 =( BOUNDED_CURVE ( )  B_SPLINE_CURVE ( 2, ( #9520, #14452, #13375, #12159, #1174, #6120, #5858, #14521, #11047 ),
 .UNSPECIFIED., .F., .F. ) 
 B_SPLINE_CURVE_WITH_KNOTS ( ( 3, 2, 2, 2, 3 ),
 ( 0.7249999999999999778, 0.7375000000000000444, 0.7500000000000000000, 0.7624999999999999556, 0.7750000000000000222 ),
 .UNSPECIFIED. ) 
 CURVE ( )  GEOMETRIC_REPRESENTATION_ITEM ( )  RATIONAL_B_SPLINE_CURVE ( ( 1.000000000000000000, 0.9238795325112867385, 1.000000000000000000, 0.9238795325112867385, 1.000000000000000000, 0.9238795325112867385, 1.000000000000000000, 0.9238795325112867385, 1.000000000000000000 ) ) 
 REPRESENTATION_ITEM ( '' )  );
#8116 = ORIENTED_EDGE ( 'NONE', *, *, #5593, .T. ) ;
#8117 = DIRECTION ( 'NONE',  ( 0.000000000000000000, 1.000000000000000000, 0.000000000000000000 ) ) ;
#8118 = VERTEX_POINT ( 'NONE', #1862 ) ;
#8119 = PRESENTATION_LAYER_ASSIGNMENT (  '', '', ( #114 ) ) ;
#8120 = LINE ( 'NONE', #7224, #13804 ) ;
#8121 = EDGE_CURVE ( 'NONE', #7289, #11317, #754, .T. ) ;
#8122 = EDGE_CURVE ( 'NONE', #3803, #1929, #15446, .T. ) ;
#8123 = EDGE_CURVE ( 'NONE', #4992, #10194, #10682, .T. ) ;
#8124 = CARTESIAN_POINT ( 'NONE',  ( 1.734723475976807094E-15, 4.618802153517012954, -0.4999999999999995559 ) ) ;
#8125 = DIRECTION ( 'NONE',  ( 0.000000000000000000, 0.000000000000000000, 1.000000000000000000 ) ) ;
#8126 = CARTESIAN_POINT ( 'NONE',  ( -3.401574460001764777, 4.209348295687701302, -8.562499997268812280 ) ) ;
#8127 = LINE ( 'NONE', #5847, #13729 ) ;
#8128 = FACE_OUTER_BOUND ( 'NONE', #14948, .T. ) ;
#8129 = CARTESIAN_POINT ( 'NONE',  ( -9.184850993605147944E-16, -25.25000000000000000, 5.000000000000000000 ) ) ;
#8130 = ORIENTED_EDGE ( 'NONE', *, *, #3235, .T. ) ;
#8131 = DIRECTION ( 'NONE',  ( 1.000000000000000000, 0.000000000000000000, 0.000000000000000000 ) ) ;
#8132 = LINE ( 'NONE', #14188, #5594 ) ;
#8133 = MECHANICAL_DESIGN_GEOMETRIC_PRESENTATION_REPRESENTATION (  '', ( #2178 ), #7620 ) ;
#8134 = ORIENTED_EDGE ( 'NONE', *, *, #12125, .T. ) ;
#8135 = DIRECTION ( 'NONE',  ( -0.9999824063907751803, -0.005931855436079011210, 0.000000000000000000 ) ) ;
#8136 = VERTEX_POINT ( 'NONE', #5513 ) ;
#8137 = VECTOR ( 'NONE', #2567, 1000.000000000000000 ) ;
#8138 = VERTEX_POINT ( 'NONE', #10442 ) ;
#8139 = CARTESIAN_POINT ( 'NONE',  ( 0.000000000000000000, 0.000000000000000000, -5.000000000000000888 ) ) ;
#8140 = CARTESIAN_POINT ( 'NONE',  ( 0.1404048886732821022, 4.699864953788070565, -3.686887068327037387 ) ) ;
#8141 = DIRECTION ( 'NONE',  ( 1.319090325525611458E-16, 1.000000000000000000, -0.000000000000000000 ) ) ;
#8142 = EDGE_CURVE ( 'NONE', #9203, #10564, #5746, .T. ) ;
#8143 = AXIS2_PLACEMENT_3D ( 'NONE', #8515, #4861, #8586 ) ;
#8144 = CARTESIAN_POINT ( 'NONE',  ( -4.209348295687703079, -3.401574460001763445, -5.437500000000002665 ) ) ;
#8145 = FACE_OUTER_BOUND ( 'NONE', #3370, .T. ) ;
#8146 = CIRCLE ( 'NONE', #1662, 2.649999999999999467 ) ;
#8147 = CARTESIAN_POINT ( 'NONE',  ( -13.27905619136138959, -35.00000000000000000, -59.00000000000000000 ) ) ;
#8148 = CARTESIAN_POINT ( 'NONE',  ( -15.99999999999979217, -9.000000000000001776, 1.499999999999998890 ) ) ;
#8149 = DIRECTION ( 'NONE',  ( -1.734723475976807686E-15, 0.000000000000000000, 1.000000000000000000 ) ) ;
#8150 = CARTESIAN_POINT ( 'NONE',  ( -9.184850993605147944E-16, -25.37500000273118417, 4.999999999999999112 ) ) ;
#8151 = CARTESIAN_POINT ( 'NONE',  ( -3.152801135295367985, -28.06250000136559564, 3.152801135295367096 ) ) ;
#8152 = CARTESIAN_POINT ( 'NONE',  ( 4.799145180956616130, -0.5093500532425063732, 0.6250000013655918618 ) ) ;
#8153 = EDGE_LOOP ( 'NONE', ( #11271, #6113 ) ) ;
#8154 = FACE_OUTER_BOUND ( 'NONE', #4645, .T. ) ;
#8155 = ORIENTED_EDGE ( 'NONE', *, *, #15691, .F. ) ;
#8156 = VERTEX_POINT ( 'NONE', #9239 ) ;
#8157 = AXIS2_PLACEMENT_3D ( 'NONE', #9306, #14229, #10518 ) ;
#8158 = CARTESIAN_POINT ( 'NONE',  ( -4.458734125000000326, -27.25000000136559564, -1.846868145590735644 ) ) ;
#8159 = CARTESIAN_POINT ( 'NONE',  ( -3.510273485745307287, -2.827716139362669967, -3.610536846335890004 ) ) ;
#8160 = VECTOR ( 'NONE', #10544, 1000.000000000000000 ) ;
#8161 = CARTESIAN_POINT ( 'NONE',  ( -1.154700538379235031, -20.00000000000000000, -34.00000000000000000 ) ) ;
#8162 = APPLICATION_CONTEXT ( 'automotive_design' ) ;
#8163 = DIRECTION ( 'NONE',  ( -1.000000000000000000, 0.000000000000000000, 0.000000000000000000 ) ) ;
#8164 = CARTESIAN_POINT ( 'NONE',  ( 2.131511515620586383, 3.916244202832140253, -4.187499998634405252 ) ) ;
#8165 = CARTESIAN_POINT ( 'NONE',  ( 0.5711823568785988625, 5.381735091635026613, -5.687499997268815832 ) ) ;
#8166 = CARTESIAN_POINT ( 'NONE',  ( -2.071067811865478170, -27.31250000000000000, 5.000000000000000000 ) ) ;
#8167 = CONICAL_SURFACE ( 'NONE', #13051, 2.041999999999999815, 1.047197551196591858 ) ;
#8168 = CARTESIAN_POINT ( 'NONE',  ( 4.209348295687701302, 3.401574460001765665, 1.062499999999996225 ) ) ;
#8169 = FACE_OUTER_BOUND ( 'NONE', #770, .T. ) ;
#8170 = CARTESIAN_POINT ( 'NONE',  ( 2.500000000000000000, 1.178949249685218525, 2.041999999999999371 ) ) ;
#8171 = CARTESIAN_POINT ( 'NONE',  ( -1.846868145590734756, -29.12500000136559919, -4.458734125000000326 ) ) ;
#8172 = AXIS2_PLACEMENT_3D ( 'NONE', #2478, #15770, #7276 ) ;
#8173 = ORIENTED_EDGE ( 'NONE', *, *, #1181, .F. ) ;
#8174 = CIRCLE ( 'NONE', #7902, 5.000000000000001776 ) ;
#8175 = CARTESIAN_POINT ( 'NONE',  ( -3.152801135295367096, -22.06250000136559564, -3.152801135295367541 ) ) ;
#8176 = DIRECTION ( 'NONE',  ( 0.000000000000000000, -0.000000000000000000, 1.000000000000000000 ) ) ;
#8177 = ORIENTED_EDGE ( 'NONE', *, *, #12035, .F. ) ;
#8178 = ORIENTED_EDGE ( 'NONE', *, *, #8757, .T. ) ;
#8179 = CARTESIAN_POINT ( 'NONE',  ( 4.795541693661363958, 1.415196051561583790, -3.874999997268816720 ) ) ;
#8180 = ADVANCED_FACE ( 'NONE', ( #6976 ), #14315, .F. ) ;
#8181 = CARTESIAN_POINT ( 'NONE',  ( -4.209348295687703079, -3.401574460001763445, -7.312499997268814944 ) ) ;
#8182 = EDGE_CURVE ( 'NONE', #13323, #5937, #9558, .T. ) ;
#8183 = AXIS2_PLACEMENT_3D ( 'NONE', #7408, #14677, #3676 ) ;
#8184 = ORIENTED_EDGE ( 'NONE', *, *, #8832, .T. ) ;
#8185 = CARTESIAN_POINT ( 'NONE',  ( -3.535533905932737309, -24.75000000273118417, -3.535533905932738197 ) ) ;
#8186 = CLOSED_SHELL ( 'NONE', ( #11457, #11195, #1897, #8884, #6005, #11456, #2467, #9196, #12602, #4360 ) ) ;
#8187 = CARTESIAN_POINT ( 'NONE',  ( -17.99999999999979394, -9.000000000000001776, -1.500000000000000888 ) ) ;
#8188 = CARTESIAN_POINT ( 'NONE',  ( -4.458734125000000326, -27.25000000136559564, -1.846868145590735644 ) ) ;
#8189 = CARTESIAN_POINT ( 'NONE',  ( -4.618802153516124775, -3.000000000000000000, -36.00000000000148503 ) ) ;
#8190 = AXIS2_PLACEMENT_3D ( 'NONE', #10629, #4557, #6757 ) ;
#8191 = DIRECTION ( 'NONE',  ( 0.000000000000000000, 0.000000000000000000, -1.000000000000000000 ) ) ;
#8192 = DIRECTION ( 'NONE',  ( 6.938893903907228378E-16, 1.000000000000000000, -0.000000000000000000 ) ) ;
#8193 = CARTESIAN_POINT ( 'NONE',  ( -28.86751345948126257, -37.00000000000000711, -50.00000000000000711 ) ) ;
#8194 = ORIENTED_EDGE ( 'NONE', *, *, #12013, .T. ) ;
#8195 = ORIENTED_EDGE ( 'NONE', *, *, #15814, .F. ) ;
#8196 =( NAMED_UNIT ( * ) SI_UNIT ( $, .STERADIAN. ) SOLID_ANGLE_UNIT ( ) );
#8198 = ORIENTED_EDGE ( 'NONE', *, *, #12086, .T. ) ;
#8197 = ADVANCED_FACE ( 'NONE', ( #4385 ), #10612, .F. ) ;
#8199 = DIRECTION ( 'NONE',  ( 1.000000000000000000, 0.000000000000000000, 0.000000000000000000 ) ) ;
#8200 = ADVANCED_FACE ( 'NONE', ( #1288, #6233 ), #8657, .F. ) ;
#8201 = ORIENTED_EDGE ( 'NONE', *, *, #13459, .F. ) ;
#8202 = CIRCLE ( 'NONE', #9978, 2.500000000000000888 ) ;
#8203 = LINE ( 'NONE', #12776, #13272 ) ;
#8204 = CARTESIAN_POINT ( 'NONE',  ( -5.000000000000004441, -7.530481206757679743E-15, -3.420263044861759916 ) ) ;
#8205 = CARTESIAN_POINT ( 'NONE',  ( -4.799145180956616130, 0.5093500532425063732, 1.125000001365592306 ) ) ;
#8206 = DIRECTION ( 'NONE',  ( 6.123233995736766036E-17, 1.000000000000000000, 0.000000000000000000 ) ) ;
#8207 = CARTESIAN_POINT ( 'NONE',  ( -0.5711823568785978633, -5.381735091635035495, -7.187499997268817609 ) ) ;
#8208 = CARTESIAN_POINT ( 'NONE',  ( -4.000000000000000000, 2.309401076758498483, -5.000000000000000000 ) ) ;
#8209 = CIRCLE ( 'NONE', #2488, 2.500000000000000888 ) ;
#8210 = CARTESIAN_POINT ( 'NONE',  ( 9.999999999999891642, -13.00000000000000178, -17.32050807568883499 ) ) ;
#8211 = DIRECTION ( 'NONE',  ( -0.000000000000000000, -1.000000000000000000, -0.000000000000000000 ) ) ;
#8212 = ORIENTED_EDGE ( 'NONE', *, *, #8757, .F. ) ;
#8213 = LINE ( 'NONE', #13112, #4077 ) ;
#8214 = CARTESIAN_POINT ( 'NONE',  ( 0.5711823568785988625, 5.381735091635026613, -2.687499997268816720 ) ) ;
#8215 =( LENGTH_UNIT ( ) NAMED_UNIT ( * ) SI_UNIT ( .MILLI., .METRE. ) );
#8216 = ADVANCED_FACE ( 'NONE', ( #6154 ), #4931, .F. ) ;
#8217 = VERTEX_POINT ( 'NONE', #13403 ) ;
#8218 = DIRECTION ( 'NONE',  ( 1.000000000000000000, 0.000000000000000000, 0.000000000000000000 ) ) ;
#8219 = EDGE_LOOP ( 'NONE', ( #6638, #5638, #4955, #2727, #7221, #12338 ) ) ;
#8220 = EDGE_CURVE ( 'NONE', #678, #15685, #3004, .T. ) ;
#8221 = VECTOR ( 'NONE', #13171, 1000.000000000000114 ) ;
#8222 = ORIENTED_EDGE ( 'NONE', *, *, #1971, .T. ) ;
#8223 = AXIS2_PLACEMENT_3D ( 'NONE', #15568, #6763, #1817 ) ;
#8224 = LINE ( 'NONE', #12366, #2482 ) ;
#8225 = DIRECTION ( 'NONE',  ( -1.000000000000000000, -0.000000000000000000, -0.000000000000000000 ) ) ;
#8226 = AXIS2_PLACEMENT_3D ( 'NONE', #5553, #10487, #5475 ) ;
#8227 = CARTESIAN_POINT ( 'NONE',  ( -5.000000000000095035, -0.7223674278660573433, -5.521799365517154889 ) ) ;
#8228 = DIRECTION ( 'NONE',  ( -0.000000000000000000, 1.000000000000000000, -0.000000000000000000 ) ) ;
#8229 = VECTOR ( 'NONE', #3597, 1000.000000000000000 ) ;
#8230 = DIRECTION ( 'NONE',  ( 0.000000000000000000, -1.000000000000000000, 0.000000000000000000 ) ) ;
#8231 = AXIS2_PLACEMENT_3D ( 'NONE', #15725, #8450, #12133 ) ;
#8232 = DIRECTION ( 'NONE',  ( 0.000000000000000000, 0.000000000000000000, 1.000000000000000000 ) ) ;
#8233 = CARTESIAN_POINT ( 'NONE',  ( -67.50000000000000000, 40.00000000000000000, -7.070249711157346244E-13 ) ) ;
#8234 = CARTESIAN_POINT ( 'NONE',  ( -28.86751345948126257, -35.00000000000000000, -50.00000000000000711 ) ) ;
#8235 = CARTESIAN_POINT ( 'NONE',  ( -3.152801135295367096, -31.31250000136559564, -3.152801135295367541 ) ) ;
#8236 = CARTESIAN_POINT ( 'NONE',  ( -3.753672977998669946, -3.033343224707661712, 0.2500000013655933606 ) ) ;
#8237 = ORIENTED_EDGE ( 'NONE', *, *, #3275, .T. ) ;
#8238 = PRESENTATION_LAYER_ASSIGNMENT (  '', '', ( #11057 ) ) ;
#8239 = CARTESIAN_POINT ( 'NONE',  ( 7.968863443239234456, 4.547634245050475421, -8.057411785091789014 ) ) ;
#8240 = ADVANCED_FACE ( 'NONE', ( #3637 ), #2341, .T. ) ;
#8241 = ORIENTED_EDGE ( 'NONE', *, *, #1440, .T. ) ;
#8242 = ORIENTED_EDGE ( 'NONE', *, *, #6490, .T. ) ;
#8243 = AXIS2_PLACEMENT_3D ( 'NONE', #1965, #1645, #6753 ) ;
#8244 = EDGE_CURVE ( 'NONE', #2510, #9721, #4690, .T. ) ;
#8245 =( NAMED_UNIT ( * ) SI_UNIT ( $, .STERADIAN. ) SOLID_ANGLE_UNIT ( ) );
#8246 = PRODUCT_DEFINITION_SHAPE ( 'NONE', 'NONE',  #15797 ) ;
#8247 = CARTESIAN_POINT ( 'NONE',  ( -1.846868145590737420, -28.00000000136559564, 4.458734124999999437 ) ) ;
#8248 = DIRECTION ( 'NONE',  ( 1.224646799147353207E-16, 1.000000000000000000, 0.000000000000000000 ) ) ;
#8249 = VECTOR ( 'NONE', #7886, 1000.000000000000000 ) ;
#8250 = VECTOR ( 'NONE', #7645, 1000.000000000000000 ) ;
#8251 = DIRECTION ( 'NONE',  ( 1.000000000000000000, 0.000000000000000000, 0.000000000000000000 ) ) ;
#8252 = CARTESIAN_POINT ( 'NONE',  ( -4.000000000000000000, 2.309401076758498483, -0.4999999999999927280 ) ) ;
#8253 = CARTESIAN_POINT ( 'NONE',  ( -4.799145180956616130, 0.5093500532425063732, -4.874999998634406140 ) ) ;
#8254 = CARTESIAN_POINT ( 'NONE',  ( 0.000000000000000000, 2.357898499370433054, -1.951563910473907981E-15 ) ) ;
#8255 = AXIS2_PLACEMENT_3D ( 'NONE', #8543, #7317, #11033 ) ;
#8256 = AXIS2_PLACEMENT_3D ( 'NONE', #2099, #7045, #7689 ) ;
#8257 = CARTESIAN_POINT ( 'NONE',  ( -2.071067811865475061, -26.68750000000000355, -5.000000000000000888 ) ) ;
#8258 = CARTESIAN_POINT ( 'NONE',  ( 2.390265326283148806, 4.391654775818395251, 1.124999999999997558 ) ) ;
#8259 = CARTESIAN_POINT ( 'NONE',  ( -41.99999999999978684, -11.00000000000000178, -1.500000000000000888 ) ) ;
#8260 = LINE ( 'NONE', #11932, #12052 ) ;
#8261 = CARTESIAN_POINT ( 'NONE',  ( 4.458734124999999437, -31.43750000136559564, 0.000000000000000000 ) ) ;
#8262 = ORIENTED_EDGE ( 'NONE', *, *, #6237, .F. ) ;
#8263 = CARTESIAN_POINT ( 'NONE',  ( 4.458734124999999437, -24.37500000136559564, -1.846868145590734978 ) ) ;
#8264 = DIRECTION ( 'NONE',  ( 0.000000000000000000, 1.000000000000000000, 0.000000000000000000 ) ) ;
#8265 = VERTEX_POINT ( 'NONE', #3470 ) ;
#8266 = ORIENTED_EDGE ( 'NONE', *, *, #10064, .F. ) ;
#8267 = CARTESIAN_POINT ( 'NONE',  ( 4.209348295687701302, 3.401574460001766109, -3.812499997268816276 ) ) ;
#8268 = ADVANCED_FACE ( 'NONE', ( #7284 ), #8582, .F. ) ;
#8269 = CARTESIAN_POINT ( 'NONE',  ( -8.190561711645485556E-16, -30.68750000136559564, 4.458734124999999437 ) ) ;
#8270 = CARTESIAN_POINT ( 'NONE',  ( -31.74999999999995737, 0.000000000000000000, 0.000000000000000000 ) ) ;
#8271 = EDGE_LOOP ( 'NONE', ( #831, #8184, #909, #3840 ) ) ;
#8273 = AXIS2_PLACEMENT_3D ( 'NONE', #6983, #8117, #13012 ) ;
#8272 = DIRECTION ( 'NONE',  ( 0.000000000000000000, 0.000000000000000000, 1.000000000000000000 ) ) ;
#8274 = PLANE ( 'NONE',  #8256 ) ;
#8275 = CARTESIAN_POINT ( 'NONE',  ( -45.00000000000000000, 0.000000000000000000, -7.500000000000000000 ) ) ;
#8276 = CARTESIAN_POINT ( 'NONE',  ( 2.730187237215162345E-16, -27.43750000136559564, -4.458734124999999437 ) ) ;
#8277 = LINE ( 'NONE', #10761, #4693 ) ;
#8278 = EDGE_CURVE ( 'NONE', #4240, #10306, #5903, .T. ) ;
#8279 = CARTESIAN_POINT ( 'NONE',  ( 6.123233995736766282E-16, -20.00000000000000000, -5.000000000000000000 ) ) ;
#8280 = CARTESIAN_POINT ( 'NONE',  ( 5.000000000000000000, -31.12500000273118772, 0.000000000000000000 ) ) ;
#8281 = LINE ( 'NONE', #904, #8221 ) ;
#8282 = VERTEX_POINT ( 'NONE', #15778 ) ;
#8283 = ORIENTED_EDGE ( 'NONE', *, *, #10428, .F. ) ;
#8284 = ORIENTED_EDGE ( 'NONE', *, *, #5320, .F. ) ;
#8285 =( REPRESENTATION_RELATIONSHIP ('NONE','NONE', #4176, #4696 ) REPRESENTATION_RELATIONSHIP_WITH_TRANSFORMATION ( #12297 )SHAPE_REPRESENTATION_RELATIONSHIP( ) );
#8286 = DIRECTION ( 'NONE',  ( 0.000000000000000000, 1.000000000000000000, -1.224646799147353207E-16 ) ) ;
#8287 = CARTESIAN_POINT ( 'NONE',  ( 0.6448876103708359731, 4.246476118072354922, -0.2256878752776725616 ) ) ;
#8288 = ADVANCED_FACE ( 'NONE', ( #9614 ), #8430, .F. ) ;
#8289 = CARTESIAN_POINT ( 'NONE',  ( 1.261996585732578113, -4.276409079477644148, -0.5624999986344088043 ) ) ;
#8290 = ADVANCED_FACE ( 'NONE', ( #1127 ), #7215, .F. ) ;
#8291 = CARTESIAN_POINT ( 'NONE',  ( -20.00000000000042633, -13.50000000000000178, -4.859237707752478708E-14 ) ) ;
#8292 = CARTESIAN_POINT ( 'NONE',  ( 3.033343224707661712, -3.753672977998669946, -2.749999998634409248 ) ) ;
#8293 = DIRECTION ( 'NONE',  ( 0.000000000000000000, 1.000000000000000000, 0.000000000000000000 ) ) ;
#8294 = DIRECTION ( 'NONE',  ( 0.000000000000000000, 0.4999999999999993339, -0.8660254037844390407 ) ) ;
#8295 = EDGE_LOOP ( 'NONE', ( #13184, #6482, #10689, #5405, #9683, #5102, #5445, #7000, #3822, #3089, #7614, #4483, #12337, #8022, #11595, #10474, #15381, #15057, #13853, #15731, #3917, #10634, #14009, #8039 ) ) ;
#8296 = DIRECTION ( 'NONE',  ( 0.8660254037844383745, 0.5000000000000004441, 0.000000000000000000 ) ) ;
#8297 = LINE ( 'NONE', #15562, #11510 ) ;
#8298 = ORIENTED_EDGE ( 'NONE', *, *, #10758, .T. ) ;
#8299 = DIRECTION ( 'NONE',  ( 0.000000000000000000, 0.000000000000000000, 1.000000000000000000 ) ) ;
#8300 = ORIENTED_EDGE ( 'NONE', *, *, #6079, .T. ) ;
#8301 = ORIENTED_EDGE ( 'NONE', *, *, #3610, .T. ) ;
#8302 = PLANE ( 'NONE',  #12710 ) ;
#8303 = CARTESIAN_POINT ( 'NONE',  ( -5.000000000000003553, 1.292545281756915047E-15, -0.4202630448617610814 ) ) ;
#8304 =( LENGTH_UNIT ( ) NAMED_UNIT ( * ) SI_UNIT ( .MILLI., .METRE. ) );
#8305 = EDGE_CURVE ( 'NONE', #2479, #6940, #13470, .T. ) ;
#8306 = CARTESIAN_POINT ( 'NONE',  ( -7.908030677224559213, 3.059924800338342354, -7.792662696733363425 ) ) ;
#8307 = CARTESIAN_POINT ( 'NONE',  ( -5.000000000000004441, -7.530481206757679743E-15, -2.545263047592944972 ) ) ;
#8308 = EDGE_CURVE ( 'NONE', #1307, #2200, #10286, .T. ) ;
#8309 = DIRECTION ( 'NONE',  ( 0.000000000000000000, 0.000000000000000000, -1.000000000000000000 ) ) ;
#8310 = CARTESIAN_POINT ( 'NONE',  ( 1.415196051561583790, -4.795541693661363958, 0.8750000027311841677 ) ) ;
#8311 = LINE ( 'NONE', #13201, #1231 ) ;
#8312 = SURFACE_SIDE_STYLE ('',( #15892 ) ) ;
#8313 = CARTESIAN_POINT ( 'NONE',  ( -1.846868145590737420, -31.00000000136559564, 4.458734124999997661 ) ) ;
#8314 = CARTESIAN_POINT ( 'NONE',  ( 3.753672977998667726, 3.033343224707664376, -0.2499999986344070280 ) ) ;
#8315 = VERTEX_POINT ( 'NONE', #11547 ) ;
#8316 = CARTESIAN_POINT ( 'NONE',  ( 0.3875187462269810701, 8.436519985397781696, -7.781689322728073677 ) ) ;
#8317 = ORIENTED_EDGE ( 'NONE', *, *, #15194, .T. ) ;
#8318 = ORIENTED_EDGE ( 'NONE', *, *, #9855, .F. ) ;
#8319 = ORIENTED_EDGE ( 'NONE', *, *, #13016, .F. ) ;
#8320 = CARTESIAN_POINT ( 'NONE',  ( 4.458734124999999437, -28.75000000136559208, 1.846868145590737864 ) ) ;
#8321 = DIRECTION ( 'NONE',  ( -0.000000000000000000, 1.000000000000000000, -0.000000000000000000 ) ) ;
#8322 = FACE_OUTER_BOUND ( 'NONE', #10054, .T. ) ;
#8323 = EDGE_CURVE ( 'NONE', #10300, #13915, #11386, .T. ) ;
#8324 = DIRECTION ( 'NONE',  ( 0.8660254037844384856, 0.000000000000000000, -0.5000000000000004441 ) ) ;
#8325 = AXIS2_PLACEMENT_3D ( 'NONE', #11795, #10837, #902 ) ;
#8326 = EDGE_CURVE ( 'NONE', #13728, #1787, #5917, .T. ) ;
#8327 = EDGE_CURVE ( 'NONE', #3134, #1476, #7992, .T. ) ;
#8328 = CARTESIAN_POINT ( 'NONE',  ( 5.000000000000000888, -22.93749999999999645, -2.071067811865475505 ) ) ;
#8329 = CARTESIAN_POINT ( 'NONE',  ( 2.131511515620586383, 3.916244202832140253, -7.187499998634407916 ) ) ;
#8330 = DIRECTION ( 'NONE',  ( 0.000000000000000000, 0.000000000000000000, 1.000000000000000000 ) ) ;
#8331 = CARTESIAN_POINT ( 'NONE',  ( -4.359993798267272069, -1.826517121560402579, -0.1962993159364725404 ) ) ;
#8332 = CARTESIAN_POINT ( 'NONE',  ( -1.846868145590737420, -29.75000000136559564, 4.458734124999999437 ) ) ;
#8333 = ORIENTED_EDGE ( 'NONE', *, *, #4109, .T. ) ;
#8334 = CARTESIAN_POINT ( 'NONE',  ( -60.00000000000000000, -37.00000000000000711, 19.99999999999999289 ) ) ;
#8335 = ORIENTED_EDGE ( 'NONE', *, *, #2948, .T. ) ;
#8336 = EDGE_LOOP ( 'NONE', ( #7683, #14304, #8863, #6495 ) ) ;
#8337 = CARTESIAN_POINT ( 'NONE',  ( -7.894706624614594048, -0.7534108004377911838, -7.590222617908730207 ) ) ;
#8338 = CARTESIAN_POINT ( 'NONE',  ( 4.458734124999999437, -30.50000000136559919, 1.846868145590737864 ) ) ;
#8339 = DIRECTION ( 'NONE',  ( 0.000000000000000000, 0.000000000000000000, 1.000000000000000000 ) ) ;
#8340 = ORIENTED_EDGE ( 'NONE', *, *, #4679, .F. ) ;
#8341 = CARTESIAN_POINT ( 'NONE',  ( 0.000000000000000000, 0.000000000000000000, -9.999999999999998224 ) ) ;
#8342 = CARTESIAN_POINT ( 'NONE',  ( 8.673617379884035472E-16, 4.618802153517012954, -5.000000000000000000 ) ) ;
#8343 = EDGE_CURVE ( 'NONE', #637, #3959, #338, .T. ) ;
#8344 = CARTESIAN_POINT ( 'NONE',  ( -3.152801135295367985, -25.06250000136559564, 3.152801135295367096 ) ) ;
#8345 = CARTESIAN_POINT ( 'NONE',  ( -44.99999999999998579, -25.00000000000000000, 17.50000000000000000 ) ) ;
#8346 = DIRECTION ( 'NONE',  ( -1.000000000000000000, -0.000000000000000000, -0.000000000000000000 ) ) ;
#8347 = CARTESIAN_POINT ( 'NONE',  ( 3.061616997868383141E-16, -30.75000000000000000, -5.000000000000000000 ) ) ;
#8348 = AXIS2_PLACEMENT_3D ( 'NONE', #8187, #3239, #11793 ) ;
#8349 = CARTESIAN_POINT ( 'NONE',  ( -3.750000000000007550, -6.495190528383289141, 0.000000000000000000 ) ) ;
#8350 = VECTOR ( 'NONE', #2370, 1000.000000000000000 ) ;
#8351 = EDGE_LOOP ( 'NONE', ( #5992, #8732, #3564, #14573 ) ) ;
#8352 = APPLICATION_PROTOCOL_DEFINITION ( 'draft international standard', 'automotive_design', 1998, #9192 ) ;
#8353 = EDGE_LOOP ( 'NONE', ( #1671, #1056, #1281, #1007, #14840, #792 ) ) ;
#8354 = ADVANCED_FACE ( 'NONE', ( #1692 ), #174, .F. ) ;
#8355 = CARTESIAN_POINT ( 'NONE',  ( -67.50000000000000000, 37.00000000000000000, -2.650000000000692690 ) ) ;
#8356 = EDGE_LOOP ( 'NONE', ( #13878, #13517, #1073, #10359 ) ) ;
#8357 = AXIS2_PLACEMENT_3D ( 'NONE', #4006, #13870, #2802 ) ;
#8358 = EDGE_CURVE ( 'NONE', #5811, #8026, #10780, .T. ) ;
#8359 = DIRECTION ( 'NONE',  ( 0.000000000000000000, 0.000000000000000000, 1.000000000000000000 ) ) ;
#8360 = CARTESIAN_POINT ( 'NONE',  ( -3.033343224707664376, 3.753672977998667726, -0.9999999986344076941 ) ) ;
#8361 = DIRECTION ( 'NONE',  ( 0.000000000000000000, -1.000000000000000000, 0.000000000000000000 ) ) ;
#8362 = PRODUCT ( 'hex flange nut gradea 1_iso_ISO - 4161 - M10 - N', 'hex flange nut gradea 1_iso_ISO - 4161 - M10 - N', '', ( #11094 ) ) ;
#8364 = VECTOR ( 'NONE', #4418, 1000.000000000000000 ) ;
#8363 = CARTESIAN_POINT ( 'NONE',  ( -4.276409079477644148, -1.261996585732578335, -2.062499998634406584 ) ) ;
#8365 = CARTESIAN_POINT ( 'NONE',  ( 0.000000000000000000, -20.00000000000000000, 5.000000000000000000 ) ) ;
#8366 = EDGE_CURVE ( 'NONE', #14589, #12457, #3953, .T. ) ;
#8367 = DIRECTION ( 'NONE',  ( 0.000000000000000000, 0.000000000000000000, 1.000000000000000000 ) ) ;
#8368 = VERTEX_POINT ( 'NONE', #4117 ) ;
#8369 = CARTESIAN_POINT ( 'NONE',  ( 0.000000000000000000, -13.00000000000000178, -25.00000000000000000 ) ) ;
#8370 = CARTESIAN_POINT ( 'NONE',  ( -60.00000000000000000, -37.00000000000000711, 19.99999999999999289 ) ) ;
#8371 = VERTEX_POINT ( 'NONE', #7606 ) ;
#8372 = CARTESIAN_POINT ( 'NONE',  ( 9.999999999999891642, -13.00000000000000178, -17.32050807568883499 ) ) ;
#8373 = VERTEX_POINT ( 'NONE', #1448 ) ;
#8374 = VERTEX_POINT ( 'NONE', #15203 ) ;
#8375 = CARTESIAN_POINT ( 'NONE',  ( 0.5093500532425063732, 4.799145180956616130, -1.374999998634406140 ) ) ;
#8376 = EDGE_CURVE ( 'NONE', #11044, #12769, #15110, .T. ) ;
#8377 = EDGE_CURVE ( 'NONE', #14100, #15134, #7527, .T. ) ;
#8378 = DIRECTION ( 'NONE',  ( 1.000000000000000000, 0.000000000000000000, 1.114413700119375779E-16 ) ) ;
#8379 = DIRECTION ( 'NONE',  ( 1.000000000000000000, 0.000000000000000000, 0.000000000000000000 ) ) ;
#8380 = CARTESIAN_POINT ( 'NONE',  ( -31.74999999999995737, 0.000000000000000000, 0.000000000000000000 ) ) ;
#8381 = DIRECTION ( 'NONE',  ( -0.000000000000000000, -1.000000000000000000, -0.000000000000000000 ) ) ;
#8382 = STYLED_ITEM ( 'NONE', ( #94 ), #6390 ) ;
#8383 = CARTESIAN_POINT ( 'NONE',  ( 6.123233995736766282E-16, -13.00000000000000178, 5.000000000000000000 ) ) ;
#8384 = DIRECTION ( 'NONE',  ( 0.000000000000000000, 0.000000000000000000, 1.000000000000000000 ) ) ;
#8385 = DIRECTION ( 'NONE',  ( 0.000000000000000000, 0.000000000000000000, 1.000000000000000000 ) ) ;
#8386 = CARTESIAN_POINT ( 'NONE',  ( 4.458734124999999437, -30.62500000136559564, -1.846868145590734978 ) ) ;
#8387 = CARTESIAN_POINT ( 'NONE',  ( -4.276409079477644148, -1.261996585732578335, 0.1875000013655918341 ) ) ;
#8388 = VERTEX_POINT ( 'NONE', #1536 ) ;
#8389 = CARTESIAN_POINT ( 'NONE',  ( -0.2791032213812753571, 8.821394357840558698, -7.929128246061909024 ) ) ;
#8390 = ORIENTED_EDGE ( 'NONE', *, *, #3783, .F. ) ;
#8391 = VERTEX_POINT ( 'NONE', #9141 ) ;
#8392 = ORIENTED_EDGE ( 'NONE', *, *, #10732, .F. ) ;
#8393 = CARTESIAN_POINT ( 'NONE',  ( -3.152801135295367096, -28.31250000136559564, -3.152801135295367541 ) ) ;
#8394 = CARTESIAN_POINT ( 'NONE',  ( -2.886751345948099789, -37.00000000000000711, -35.00000000000000000 ) ) ;
#8395 = B_SPLINE_CURVE_WITH_KNOTS ( 'NONE', 3,
 ( #14876, #11151, #1367, #2492, #176, #6314, #15853, #8584, #10913, #16 ),
 .UNSPECIFIED., .F., .F.,
 ( 4, 2, 2, 2, 4 ),
 ( 0.000000000000000000, 0.002305503304226492935, 0.004611006608452985871, 0.006916509912679477505, 0.009222013216905968272 ),
 .UNSPECIFIED. ) ;
#8396 = EDGE_CURVE ( 'NONE', #10919, #11587, #11229, .T. ) ;
#8397 = PRESENTATION_LAYER_ASSIGNMENT (  '', '', ( #15362 ) ) ;
#8398 = CYLINDRICAL_SURFACE ( 'NONE', #4505, 5.000000000000000888 ) ;
#8399 = CIRCLE ( 'NONE', #14572, 2.499999999999998668 ) ;
#8400 = SPHERICAL_SURFACE ( 'NONE', #7404, 10.00000000000000000 ) ;
#8401 = CARTESIAN_POINT ( 'NONE',  ( 2.071067811865475505, -23.81250000000000000, -5.000000000000000888 ) ) ;
#8402 = CARTESIAN_POINT ( 'NONE',  ( -4.391654775818395251, 2.390265326283148806, 0.3749999999999968914 ) ) ;
#8403 = CARTESIAN_POINT ( 'NONE',  ( 3.401574460001763445, -4.209348295687703079, -2.062499997268814500 ) ) ;
#8404 = LINE ( 'NONE', #13296, #4067 ) ;
#8405 = CARTESIAN_POINT ( 'NONE',  ( 2.730187237215162345E-16, -30.18750000136559564, -4.458734124999999437 ) ) ;
#8406 = CIRCLE ( 'NONE', #1709, 75.00000000000004263 ) ;
#8407 = B_SPLINE_CURVE_WITH_KNOTS ( 'NONE', 3,
 ( #2652, #408, #15035, #10023, #334, #14960, #15276, #10270, #11541, #5331, #1769, #11308, #3875, #9136, #5174, #8817, #6716, #13719 ),
 .UNSPECIFIED., .F., .F.,
 ( 4, 2, 2, 2, 2, 2, 2, 2, 4 ),
 ( 0.0005803541179376217390, 0.001389229044063926190, 0.002198103970190230967, 0.003006978896316535744, 0.003815853822442840087, 0.004624728748569143996, 0.005433603674695449207, 0.006242478600821752682, 0.007051353526948056158 ),
 .UNSPECIFIED. ) ;
#8408 = CARTESIAN_POINT ( 'NONE',  ( 3.916244202832140253, -2.131511515620588160, 1.312500001365592750 ) ) ;
#8409 = ORIENTED_EDGE ( 'NONE', *, *, #1571, .T. ) ;
#8410 = AXIS2_PLACEMENT_3D ( 'NONE', #2351, #3244, #4456 ) ;
#8411 = CARTESIAN_POINT ( 'NONE',  ( 2.500000000000000000, 3.004629197474318851E-15, 2.042000000000000259 ) ) ;
#8412 = ORIENTED_EDGE ( 'NONE', *, *, #5503, .T. ) ;
#8413 = ORIENTED_EDGE ( 'NONE', *, *, #2974, .T. ) ;
#8414 = DIRECTION ( 'NONE',  ( -0.9396926207859143121, 0.000000000000000000, -0.3420201433256525592 ) ) ;
#8415 = CARTESIAN_POINT ( 'NONE',  ( -3.152801135295367985, -28.81250000136559564, 3.152801135295367096 ) ) ;
#8416 = ADVANCED_FACE ( 'NONE', ( #12429 ), #6698, .F. ) ;
#8417 = DIRECTION ( 'NONE',  ( -0.000000000000000000, -0.000000000000000000, 1.000000000000000000 ) ) ;
#8418 = EDGE_CURVE ( 'NONE', #6759, #2789, #11464, .T. ) ;
#8419 = EDGE_CURVE ( 'NONE', #4440, #13915, #4335, .T. ) ;
#8420 = ORIENTED_EDGE ( 'NONE', *, *, #5114, .T. ) ;
#8421 = CARTESIAN_POINT ( 'NONE',  ( 42.02221399786069611, 0.000000000000000000, 2.650000000000100275 ) ) ;
#8422 = AXIS2_PLACEMENT_3D ( 'NONE', #3314, #8264, #3384 ) ;
#8423 = CARTESIAN_POINT ( 'NONE',  ( -44.99999999999999289, -13.00000000000000178, 4.000000000000831335 ) ) ;
#8424 = CARTESIAN_POINT ( 'NONE',  ( -2.000000000000007550, -3.464101615137749945, 0.000000000000000000 ) ) ;
#8425 = DIRECTION ( 'NONE',  ( 0.000000000000000000, 0.000000000000000000, -1.000000000000000000 ) ) ;
#8426 = TOROIDAL_SURFACE ( 'NONE', #8934, 2.700000000000001066, 0.2000000000000000111 ) ;
#8427 = CARTESIAN_POINT ( 'NONE',  ( -8.190561711645485556E-16, -22.93750000136559564, 4.458734124999999437 ) ) ;
#8428 = AXIS2_PLACEMENT_3D ( 'NONE', #15925, #9849, #15772 ) ;
#8429 = CARTESIAN_POINT ( 'NONE',  ( 2.836893136758676270, 3.208949435745843903, -3.505054077164911241 ) ) ;
#8430 = CYLINDRICAL_SURFACE ( 'NONE', #211, 2.499999999999998668 ) ;
#8431 = CARTESIAN_POINT ( 'NONE',  ( -91.33974596215558961, -99.99999999999994316, -7.500000000000000000 ) ) ;
#8432 = DIRECTION ( 'NONE',  ( 0.000000000000000000, 0.000000000000000000, 1.000000000000000000 ) ) ;
#8433 = ORIENTED_EDGE ( 'NONE', *, *, #15270, .F. ) ;
#8434 = AXIS2_PLACEMENT_3D ( 'NONE', #15344, #3132, #636 ) ;
#8435 = ORIENTED_EDGE ( 'NONE', *, *, #2261, .T. ) ;
#8436 = CARTESIAN_POINT ( 'NONE',  ( 42.02221399786069611, 0.000000000000000000, 2.650000000000096723 ) ) ;
#8437 = AXIS2_PLACEMENT_3D ( 'NONE', #2814, #13713, #2646 ) ;
#8438 = ADVANCED_FACE ( 'NONE', ( #262 ), #5177, .T. ) ;
#8439 = ORIENTED_EDGE ( 'NONE', *, *, #15270, .T. ) ;
#8440 = DIRECTION ( 'NONE',  ( 0.000000000000000000, 1.000000000000000000, 0.000000000000000000 ) ) ;
#8441 = VECTOR ( 'NONE', #5533, 1000.000000000000000 ) ;
#8442 = CARTESIAN_POINT ( 'NONE',  ( -4.000000000000000000, 2.309401076758498483, -3.433295621305379353 ) ) ;
#8443 = CARTESIAN_POINT ( 'NONE',  ( 4.799145180956616130, -0.5093500532425063732, -0.3749999986344090264 ) ) ;
#8444 = DIRECTION ( 'NONE',  ( -0.000000000000000000, -1.000000000000000000, -0.000000000000000000 ) ) ;
#8445 = CIRCLE ( 'NONE', #8688, 2.649999999999992806 ) ;
#8446 = CARTESIAN_POINT ( 'NONE',  ( 4.276409079477644148, 1.261996585732577891, -1.562499998634406140 ) ) ;
#8447 = AXIS2_PLACEMENT_3D ( 'NONE', #8454, #13349, #7240 ) ;
#8448 = CARTESIAN_POINT ( 'NONE',  ( 0.5974722283283607771, -8.315303285985692128, -0.7026937717022981866 ) ) ;
#8449 = EDGE_LOOP ( 'NONE', ( #663, #439 ) ) ;
#8450 = DIRECTION ( 'NONE',  ( 0.000000000000000000, -0.8660254037844390407, -0.4999999999999994449 ) ) ;
#8451 = VERTEX_POINT ( 'NONE', #6474 ) ;
#8452 = CARTESIAN_POINT ( 'NONE',  ( 4.391654775818395251, -2.390265326283149694, -1.125000000000000888 ) ) ;
#8453 = AXIS2_PLACEMENT_3D ( 'NONE', #5154, #13698, #2710 ) ;
#8454 = CARTESIAN_POINT ( 'NONE',  ( -19.99999999999956657, -9.000000000000001776, 8.786575603324269439E-13 ) ) ;
#8455 = ORIENTED_EDGE ( 'NONE', *, *, #8484, .F. ) ;
#8456 = CARTESIAN_POINT ( 'NONE',  ( 4.799145180956616130, -0.5093500532425063732, -3.624999998634407916 ) ) ;
#8457 = VECTOR ( 'NONE', #13700, 1000.000000000000000 ) ;
#8458 = DIRECTION ( 'NONE',  ( -1.000000000000000000, 0.000000000000000000, -0.000000000000000000 ) ) ;
#8459 = CARTESIAN_POINT ( 'NONE',  ( 0.000000000000000000, 20.00000000000000000, 0.000000000000000000 ) ) ;
#8461 = DIRECTION ( 'NONE',  ( 0.5000000000000004441, 0.8660254037844383745, 0.000000000000000000 ) ) ;
#8460 = CIRCLE ( 'NONE', #9479, 1.999999999999998224 ) ;
#8462 = FACE_OUTER_BOUND ( 'NONE', #13084, .T. ) ;
#8463 = CARTESIAN_POINT ( 'NONE',  ( 0.5711823568785989735, 5.381735091635026613, -1.687499997268816054 ) ) ;
#8464 = DIRECTION ( 'NONE',  ( -0.8660254037844389297, -0.000000000000000000, 0.4999999999999997780 ) ) ;
#8465 = ADVANCED_FACE ( 'NONE', ( #15038 ), #8897, .F. ) ;
#8466 = CARTESIAN_POINT ( 'NONE',  ( -4.458734124999999437, -26.18750000136559919, -5.460374474430324690E-16 ) ) ;
#8467 = CARTESIAN_POINT ( 'NONE',  ( 1.261996585732578113, -4.276409079477644148, -4.562499998634405252 ) ) ;
#8468 = VECTOR ( 'NONE', #13321, 1000.000000000000000 ) ;
#8469 = CARTESIAN_POINT ( 'NONE',  ( -28.86751345948126257, -37.00000000000000711, -50.00000000000000711 ) ) ;
#8470 = VERTEX_POINT ( 'NONE', #12668 ) ;
#8471 = ORIENTED_EDGE ( 'NONE', *, *, #5019, .F. ) ;
#8472 = ORIENTED_EDGE ( 'NONE', *, *, #9830, .T. ) ;
#8473 = CARTESIAN_POINT ( 'NONE',  ( -1.846868145590734756, -24.37500000136559564, -4.458734125000000326 ) ) ;
#8474 = VECTOR ( 'NONE', #5251, 1000.000000000000000 ) ;
#8475 = DIRECTION ( 'NONE',  ( 0.000000000000000000, 0.000000000000000000, 1.000000000000000000 ) ) ;
#8476 = CARTESIAN_POINT ( 'NONE',  ( 0.000000000000000000, 40.00000000000000000, 0.000000000000000000 ) ) ;
#8477 = AXIS2_PLACEMENT_3D ( 'NONE', #13831, #3971, #8922 ) ;
#8478 = CARTESIAN_POINT ( 'NONE',  ( -91.33974596215558961, -105.7735026918962404, -7.500000000000001776 ) ) ;
#8479 = CARTESIAN_POINT ( 'NONE',  ( 9.999999999999891642, -20.00000000000000000, -14.82050807568883677 ) ) ;
#8480 = CARTESIAN_POINT ( 'NONE',  ( -3.535533905932737309, -22.62500000000000000, -3.535533905932738197 ) ) ;
#8481 = CARTESIAN_POINT ( 'NONE',  ( -4.391654775818395251, 2.390265326283148806, -2.625000000000002220 ) ) ;
#8482 = CARTESIAN_POINT ( 'NONE',  ( -0.5711823568785977523, -5.381735091635034607, -2.187499997268816276 ) ) ;
#8483 = AXIS2_PLACEMENT_3D ( 'NONE', #4254, #14119, #3046 ) ;
#8484 = EDGE_CURVE ( 'NONE', #1698, #5598, #6549, .T. ) ;
#8485 = CARTESIAN_POINT ( 'NONE',  ( -4.671041856245029322, -9.682850088987660890E-14, -0.2303389720127052009 ) ) ;
#8486 = EDGE_CURVE ( 'NONE', #11087, #15683, #3147, .T. ) ;
#8487 = CARTESIAN_POINT ( 'NONE',  ( 4.458734124999999437, -28.43750000136559564, 0.000000000000000000 ) ) ;
#8488 = AXIS2_PLACEMENT_3D ( 'NONE', #14898, #5115, #11167 ) ;
#8489 = CARTESIAN_POINT ( 'NONE',  ( -0.5093500532425060401, -4.799145180956616130, -2.874999998634407472 ) ) ;
#8490 = VERTEX_POINT ( 'NONE', #15596 ) ;
#8491 = FACE_OUTER_BOUND ( 'NONE', #5680, .T. ) ;
#8492 = VERTEX_POINT ( 'NONE', #6959 ) ;
#8493 = EDGE_LOOP ( 'NONE', ( #38, #268, #5508, #11280 ) ) ;
#8494 = DIRECTION ( 'NONE',  ( 1.239088197126290570E-16, -0.000000000000000000, 1.000000000000000000 ) ) ;
#8495 = AXIS2_PLACEMENT_3D ( 'NONE', #14253, #9255, #2114 ) ;
#8496 = CARTESIAN_POINT ( 'NONE',  ( 1.846868145590736310, -23.62500000136559919, 4.458734124999999437 ) ) ;
#8497 = CARTESIAN_POINT ( 'NONE',  ( -28.86751345948196601, 1.999999999999998224, -75.00199999999976797 ) ) ;
#8498 = ORIENTED_EDGE ( 'NONE', *, *, #1935, .F. ) ;
#8499 = DIRECTION ( 'NONE',  ( 0.000000000000000000, 0.000000000000000000, 1.000000000000000000 ) ) ;
#8500 = VECTOR ( 'NONE', #9469, 1000.000000000000000 ) ;
#8501 = AXIS2_PLACEMENT_3D ( 'NONE', #6469, #11223, #2650 ) ;
#8502 = PRODUCT ( 'Mounting Flange Plate', 'Mounting Flange Plate', '', ( #12851 ) ) ;
#8503 = CARTESIAN_POINT ( 'NONE',  ( 3.535533905932736864, -22.12500000000000000, 3.535533905932738641 ) ) ;
#8504 = LINE ( 'NONE', #3632, #3825 ) ;
#8505 = DIRECTION ( 'NONE',  ( 0.9999824063907751803, 0.005931855436079011210, -0.000000000000000000 ) ) ;
#8506 = CARTESIAN_POINT ( 'NONE',  ( 3.152801135295366208, -21.81250000136559208, 3.152801135295367985 ) ) ;
#8507 = CIRCLE ( 'NONE', #10572, 32.00000000000000000 ) ;
#8508 = FACE_OUTER_BOUND ( 'NONE', #3115, .T. ) ;
#8509 = EDGE_CURVE ( 'NONE', #12023, #10516, #7182, .T. ) ;
#8510 = CARTESIAN_POINT ( 'NONE',  ( 0.000000000000000000, 0.000000000000000000, -25.03750572909317285 ) ) ;
#8511 = EDGE_CURVE ( 'NONE', #509, #1411, #8725, .T. ) ;
#8512 = SURFACE_STYLE_USAGE ( .BOTH. , #3330 ) ;
#8513 = CARTESIAN_POINT ( 'NONE',  ( 0.000000000000000000, -13.00000000000000178, -1.500000000000000000 ) ) ;
#8514 = LINE ( 'NONE', #984, #14648 ) ;
#8515 = CARTESIAN_POINT ( 'NONE',  ( -67.50000000000000000, 50.00000000000000000, -7.070249711157346244E-13 ) ) ;
#8516 = EDGE_LOOP ( 'NONE', ( #989, #4682, #12253, #2075 ) ) ;
#8517 = ORIENTED_EDGE ( 'NONE', *, *, #3556, .T. ) ;
#8518 = CARTESIAN_POINT ( 'NONE',  ( -90.00000000000000000, -35.00000000000000000, 13.35786437626905077 ) ) ;
#8519 = VERTEX_POINT ( 'NONE', #9449 ) ;
#8520 = FACE_OUTER_BOUND ( 'NONE', #10647, .T. ) ;
#8521 = CARTESIAN_POINT ( 'NONE',  ( 0.000000000000000000, 0.000000000000000000, 0.000000000000000000 ) ) ;
#8522 = CARTESIAN_POINT ( 'NONE',  ( -3.033343224707664376, 3.753672977998667726, 1.365593156898739876E-09 ) ) ;
#8523 = DIRECTION ( 'NONE',  ( 0.9591083387322728582, 0.000000000000000000, -0.2830392103123166025 ) ) ;
#8524 = ADVANCED_FACE ( 'NONE', ( #1773 ), #9526, .T. ) ;
#8525 = CARTESIAN_POINT ( 'NONE',  ( 1.261996585732578113, -4.276409079477644148, -1.812499998634406584 ) ) ;
#8526 = DIRECTION ( 'NONE',  ( 0.000000000000000000, 0.000000000000000000, 1.000000000000000000 ) ) ;
#8527 = SURFACE_STYLE_FILL_AREA ( #9563 ) ;
#8528 = ORIENTED_EDGE ( 'NONE', *, *, #13280, .T. ) ;
#8529 = CARTESIAN_POINT ( 'NONE',  ( 2.500000000000000000, 0.000000000000000000, 0.000000000000000000 ) ) ;
#8530 = ORIENTED_EDGE ( 'NONE', *, *, #15439, .T. ) ;
#8531 = CARTESIAN_POINT ( 'NONE',  ( 3.401574460001763445, -4.209348295687703079, -1.187500000000001998 ) ) ;
#8532 = ORIENTED_EDGE ( 'NONE', *, *, #8862, .F. ) ;
#8533 = EDGE_LOOP ( 'NONE', ( #2185, #15602, #12196, #15642 ) ) ;
#8534 = ORIENTED_EDGE ( 'NONE', *, *, #11068, .T. ) ;
#8535 = CARTESIAN_POINT ( 'NONE',  ( 2.131511515620586383, 3.916244202832140253, -3.437499998634407916 ) ) ;
#8536 =( BOUNDED_SURFACE ( )  B_SPLINE_SURFACE ( 3, 2, ( 
 ( #10267, #405, #11455 ),
 ( #2816, #10345, #8891 ),
 ( #3945, #5410, #14955 ),
 ( #13716, #5241, #14044 ),
 ( #5084, #13793, #5327 ),
 ( #15103, #9057, #12737 ) ),
 .UNSPECIFIED., .F., .F., .F. ) 
 B_SPLINE_SURFACE_WITH_KNOTS ( ( 4, 2, 4 ),
 ( 3, 3 ),
 ( 0.02032853247518126918, 0.02278863295364821906, 0.02524873343211517240 ),
 ( 0.000000000000000000, 1.000000000000000000 ),
 .UNSPECIFIED. ) 
 GEOMETRIC_REPRESENTATION_ITEM ( )  RATIONAL_B_SPLINE_SURFACE ( (
 ( 1.000000000000000000, 0.8047781615896837382, 1.000000000000000000),
 ( 1.000000000000000000, 0.8123767586289252218, 1.000000000000000000),
 ( 1.000000000000000000, 0.8190662415564388121, 1.000000000000000000),
 ( 1.000000000000000000, 0.8192361015669026303, 1.000000000000000000),
 ( 1.000000000000000000, 0.8126135807103900266, 1.000000000000000000),
 ( 1.000000000000000000, 0.8047712338318593339, 1.000000000000000000) ) ) 
 REPRESENTATION_ITEM ( '' )  SURFACE ( )  );
#8537 = CARTESIAN_POINT ( 'NONE',  ( -19.99999999999956657, -9.000000000000001776, 8.786575603324269439E-13 ) ) ;
#8538 = CARTESIAN_POINT ( 'NONE',  ( -9.184850993605147944E-16, -27.37500000273118772, 5.000000000000000000 ) ) ;
#8539 = DIRECTION ( 'NONE',  ( 0.000000000000000000, 1.000000000000000000, 0.000000000000000000 ) ) ;
#8540 = DIRECTION ( 'NONE',  ( -0.5000000000000008882, -0.8660254037844382635, 0.000000000000000000 ) ) ;
#8541 = EDGE_CURVE ( 'NONE', #2810, #8470, #7955, .T. ) ;
#8542 = B_SPLINE_CURVE_WITH_KNOTS ( 'NONE', 3,
 ( #1273, #6218, #8641, #7677, #14857, #3778, #4916, #9763 ),
 .UNSPECIFIED., .F., .F.,
 ( 4, 2, 2, 4 ),
 ( 0.006061689441712453386, 0.007174127271521678166, 0.008286565101330902947, 0.01051144076094935077 ),
 .UNSPECIFIED. ) ;
#8543 = CARTESIAN_POINT ( 'NONE',  ( 0.000000000000000000, -20.00000000000000000, 0.000000000000000000 ) ) ;
#8544 = CARTESIAN_POINT ( 'NONE',  ( -4.795541693661363958, -1.415196051561583790, -0.3749999972688169980 ) ) ;
#8545 = DIRECTION ( 'NONE',  ( -1.000000000000000000, -0.000000000000000000, -0.000000000000000000 ) ) ;
#8546 = CARTESIAN_POINT ( 'NONE',  ( 1.846868145590736310, -25.87500000136559564, 4.458734124999997661 ) ) ;
#8547 = CARTESIAN_POINT ( 'NONE',  ( 4.458734124999999437, -22.37500000136559564, -1.846868145590734978 ) ) ;
#8548 = CARTESIAN_POINT ( 'NONE',  ( 2.131511515620586383, 3.916244202832140253, -5.187499998634406140 ) ) ;
#8549 = DIRECTION ( 'NONE',  ( 0.4999999999999998335, 0.000000000000000000, 0.8660254037844387076 ) ) ;
#8550 = ORIENTED_EDGE ( 'NONE', *, *, #12160, .F. ) ;
#8551 = ORIENTED_EDGE ( 'NONE', *, *, #7275, .T. ) ;
#8552 = ORIENTED_EDGE ( 'NONE', *, *, #2281, .T. ) ;
#8553 = CARTESIAN_POINT ( 'NONE',  ( 1.846868145590736310, -22.87500000136559564, 4.458734124999999437 ) ) ;
#8554 = CYLINDRICAL_SURFACE ( 'NONE', #7915, 2.649999999999992806 ) ;
#8555 = DIRECTION ( 'NONE',  ( 0.000000000000000000, -1.000000000000000000, 0.000000000000000000 ) ) ;
#8556 = EDGE_CURVE ( 'NONE', #6278, #9986, #11779, .T. ) ;
#8557 = DIRECTION ( 'NONE',  ( 0.4999999999999960032, 0.8660254037844409281, 0.000000000000000000 ) ) ;
#8558 = DIRECTION ( 'NONE',  ( 0.000000000000000000, 1.000000000000000000, 0.000000000000000000 ) ) ;
#8559 = CARTESIAN_POINT ( 'NONE',  ( 3.535533905932738197, -22.87500000000000000, -3.535533905932738197 ) ) ;
#8560 = CARTESIAN_POINT ( 'NONE',  ( -4.209348295687703967, -3.401574460001763001, 0.5624999999999957812 ) ) ;
#8561 = CARTESIAN_POINT ( 'NONE',  ( -5.000000000000004441, -7.530481206757679743E-15, -2.420263044861759472 ) ) ;
#8562 = LINE ( 'NONE', #8637, #2009 ) ;
#8563 = CARTESIAN_POINT ( 'NONE',  ( -4.458734125000000326, -26.00000000136559208, -1.846868145590735644 ) ) ;
#8564 = CARTESIAN_POINT ( 'NONE',  ( -4.799145180956616130, 0.5093500532425063732, -2.124999998634406584 ) ) ;
#8565 = ORIENTED_EDGE ( 'NONE', *, *, #13908, .F. ) ;
#8566 = DIRECTION ( 'NONE',  ( -1.000000000000000000, 0.000000000000000000, 0.000000000000000000 ) ) ;
#8567 = ORIENTED_EDGE ( 'NONE', *, *, #12775, .F. ) ;
#8568 = ORIENTED_EDGE ( 'NONE', *, *, #13110, .T. ) ;
#8569 = LINE ( 'NONE', #15768, #14957 ) ;
#8570 = CARTESIAN_POINT ( 'NONE',  ( -4.458734125000000326, -24.00000000136559564, -1.846868145590735644 ) ) ;
#8571 = CARTESIAN_POINT ( 'NONE',  ( -28.86751345948128744, -35.00000000000000000, 17.99999999999999645 ) ) ;
#8572 = ORIENTED_EDGE ( 'NONE', *, *, #15904, .T. ) ;
#8573 = DIRECTION ( 'NONE',  ( -0.000000000000000000, 1.000000000000000000, -0.000000000000000000 ) ) ;
#8574 = EDGE_CURVE ( 'NONE', #12974, #5996, #8260, .T. ) ;
#8575 = EDGE_CURVE ( 'NONE', #15092, #8265, #9246, .T. ) ;
#8576 = CARTESIAN_POINT ( 'NONE',  ( 2.467663300281918126E-15, 37.00000000000000000, -64.85000000000002274 ) ) ;
#8577 = CARTESIAN_POINT ( 'NONE',  ( 4.211140560182196957, 2.431303136016536470, -3.745885042887433514 ) ) ;
#8578 = DIRECTION ( 'NONE',  ( 0.000000000000000000, 0.000000000000000000, 1.000000000000000000 ) ) ;
#8579 = CARTESIAN_POINT ( 'NONE',  ( 4.458734124999999437, -21.68750000136559208, 0.000000000000000000 ) ) ;
#8580 = CARTESIAN_POINT ( 'NONE',  ( -2.886751345948130432, -5.000000000000000000, 35.00000000000001421 ) ) ;
#8581 =( REPRESENTATION_RELATIONSHIP ('NONE','NONE', #4176, #396 ) REPRESENTATION_RELATIONSHIP_WITH_TRANSFORMATION ( #12685 )SHAPE_REPRESENTATION_RELATIONSHIP( ) );
#8582 = CYLINDRICAL_SURFACE ( 'NONE', #10046, 5.000000000000000888 ) ;
#8583 = CARTESIAN_POINT ( 'NONE',  ( -2.071067811865475061, -27.81250000273118772, -5.000000000000000888 ) ) ;
#8584 = CARTESIAN_POINT ( 'NONE',  ( 6.602753909532903087, 5.319290460493538042, -7.792447862505328615 ) ) ;
#8585 = CARTESIAN_POINT ( 'NONE',  ( -3.152801135295367985, -30.81250000136559564, 3.152801135295367096 ) ) ;
#8586 = DIRECTION ( 'NONE',  ( 0.000000000000000000, 0.000000000000000000, 1.000000000000000000 ) ) ;
#8587 = ORIENTED_EDGE ( 'NONE', *, *, #63, .T. ) ;
#8588 = ORIENTED_EDGE ( 'NONE', *, *, #14291, .T. ) ;
#8589 = DIRECTION ( 'NONE',  ( 0.000000000000000000, 1.000000000000000000, 0.000000000000000000 ) ) ;
#8590 = VERTEX_POINT ( 'NONE', #7032 ) ;
#8591 = CARTESIAN_POINT ( 'NONE',  ( 0.000000000000000000, 2.357898499370433054, -1.951563910473907981E-15 ) ) ;
#8592 = EDGE_CURVE ( 'NONE', #9570, #2381, #5803, .T. ) ;
#8593 = DIRECTION ( 'NONE',  ( -0.000000000000000000, -0.000000000000000000, -1.000000000000000000 ) ) ;
#8594 = CIRCLE ( 'NONE', #14523, 4.250000000000000000 ) ;
#8595 = CARTESIAN_POINT ( 'NONE',  ( -4.799145180956616130, 0.5093500532425063732, -2.874999998634407472 ) ) ;
#8596 = PRODUCT_CONTEXT ( 'NONE', #14240, 'mechanical' ) ;
#8597 = CARTESIAN_POINT ( 'NONE',  ( -3.753672977998669946, -3.033343224707661712, -0.9999999986344076941 ) ) ;
#8598 = DIRECTION ( 'NONE',  ( 0.000000000000000000, 0.000000000000000000, 1.000000000000000000 ) ) ;
#8599 = CARTESIAN_POINT ( 'NONE',  ( -21.01110699893060030, 0.000000000000000000, 33.74230484541324415 ) ) ;
#8600 = EDGE_LOOP ( 'NONE', ( #12596, #8882, #2641, #6684, #5679 ) ) ;
#8601 = DIRECTION ( 'NONE',  ( -1.000000000000000000, 0.000000000000000000, 0.000000000000000000 ) ) ;
#8602 = DIRECTION ( 'NONE',  ( 0.000000000000000000, 0.000000000000000000, -1.000000000000000000 ) ) ;
#8603 = CONICAL_SURFACE ( 'NONE', #1626, 4.174999999999999822, 0.9599310885968795892 ) ;
#8604 = EDGE_LOOP ( 'NONE', ( #7705, #12102, #827, #2961 ) ) ;
#8605 = CARTESIAN_POINT ( 'NONE',  ( -4.276409079477644148, -1.261996585732578335, -4.062499998634405252 ) ) ;
#8606 = EDGE_CURVE ( 'NONE', #15795, #3371, #807, .T. ) ;
#8607 = AXIS2_PLACEMENT_3D ( 'NONE', #648, #3217, #11928 ) ;
#8608 = EDGE_CURVE ( 'NONE', #5764, #13099, #12911, .T. ) ;
#8609 = EDGE_CURVE ( 'NONE', #10728, #14880, #12575, .T. ) ;
#8610 = B_SPLINE_CURVE_WITH_KNOTS ( 'NONE', 3,
 ( #12605, #13735, #1703, #5509, #12758, #1548 ),
 .UNSPECIFIED., .F., .F.,
 ( 4, 2, 4 ),
 ( 0.004615310220740744332, 0.006918661718823354567, 0.009222013216905964803 ),
 .UNSPECIFIED. ) ;
#8611 = CARTESIAN_POINT ( 'NONE',  ( 4.000000000000000000, 0.1981133338132474442, 2.382280164152719704E-17 ) ) ;
#8612 = DIRECTION ( 'NONE',  ( 0.000000000000000000, 0.000000000000000000, 1.000000000000000000 ) ) ;
#8613 = AXIS2_PLACEMENT_3D ( 'NONE', #10002, #9756, #2466 ) ;
#8614 = DIRECTION ( 'NONE',  ( 0.000000000000000000, 1.000000000000000000, -1.471414886128461471E-15 ) ) ;
#8615 = DIRECTION ( 'NONE',  ( 0.000000000000000000, 0.000000000000000000, 1.000000000000000000 ) ) ;
#8616 = CARTESIAN_POINT ( 'NONE',  ( -5.000000000000000888, -30.68750000273118772, -2.071067811865475949 ) ) ;
#8617 = DIRECTION ( 'NONE',  ( 0.000000000000000000, 0.000000000000000000, 1.000000000000000000 ) ) ;
#8618 = DIRECTION ( 'NONE',  ( -1.000000000000000000, 0.000000000000000000, -0.000000000000000000 ) ) ;
#8619 = CARTESIAN_POINT ( 'NONE',  ( -4.458734124999999437, -24.18750000136559564, -5.460374474430324690E-16 ) ) ;
#8620 = CARTESIAN_POINT ( 'NONE',  ( 3.152801135295367541, -22.31250000136559564, -3.152801135295367541 ) ) ;
#8621 = CARTESIAN_POINT ( 'NONE',  ( 3.753672977998667726, 3.033343224707664376, -3.249999998634409692 ) ) ;
#8622 = FACE_OUTER_BOUND ( 'NONE', #12232, .T. ) ;
#8623 = EDGE_LOOP ( 'NONE', ( #12715, #8912 ) ) ;
#8624 = ORIENTED_EDGE ( 'NONE', *, *, #8509, .F. ) ;
#8625 =( BOUNDED_CURVE ( )  B_SPLINE_CURVE ( 2, ( #7142, #12045, #5924, #4543, #15713, #14413, #2275, #10922, #4628 ),
 .UNSPECIFIED., .F., .F. ) 
 B_SPLINE_CURVE_WITH_KNOTS ( ( 3, 2, 2, 2, 3 ),
 ( 0.5250000000000001332, 0.5375000000000000888, 0.5500000000000000444, 0.5625000000000000000, 0.5749999999999998446 ),
 .UNSPECIFIED. ) 
 CURVE ( )  GEOMETRIC_REPRESENTATION_ITEM ( )  RATIONAL_B_SPLINE_CURVE ( ( 0.9999999999999993339, 0.9238795325112874046, 1.000000000000000000, 0.9238795325112867385, 1.000000000000000000, 0.9238795325112867385, 1.000000000000000000, 0.9238795325112874046, 0.9999999999999993339 ) ) 
 REPRESENTATION_ITEM ( '' )  );
#8626 = CARTESIAN_POINT ( 'NONE',  ( 0.000000000000000000, 0.000000000000000000, 0.000000000000000000 ) ) ;
#8627 = ORIENTED_EDGE ( 'NONE', *, *, #8541, .T. ) ;
#8628 = CARTESIAN_POINT ( 'NONE',  ( 4.458734124999999437, -21.68750000136559208, 0.000000000000000000 ) ) ;
#8629 = DIRECTION ( 'NONE',  ( 0.000000000000000000, 0.000000000000000000, -1.000000000000000000 ) ) ;
#8630 = EDGE_CURVE ( 'NONE', #15938, #3118, #14653, .T. ) ;
#8631 = CARTESIAN_POINT ( 'NONE',  ( -2.071067811865468400, -27.81250000273118772, -5.000000000000007994 ) ) ;
#8632 = STYLED_ITEM ( 'NONE', ( #756 ), #608 ) ;
#8633 = DIRECTION ( 'NONE',  ( 0.000000000000000000, 0.000000000000000000, -1.000000000000000000 ) ) ;
#8634 = DIRECTION ( 'NONE',  ( -1.000000000000000000, -0.000000000000000000, -3.343241100358131282E-16 ) ) ;
#8635 = CARTESIAN_POINT ( 'NONE',  ( -5.000000000000000888, -23.43749999999999645, 2.071067811865474617 ) ) ;
#8636 = CARTESIAN_POINT ( 'NONE',  ( 3.401574460001763001, -4.209348295687703967, -0.1875000000000048572 ) ) ;
#8637 = CARTESIAN_POINT ( 'NONE',  ( 31.75426480542940766, -37.00000000000000711, 15.00000000000001066 ) ) ;
#8638 = CARTESIAN_POINT ( 'NONE',  ( 4.458734124999999437, -28.50000000136559564, 1.846868145590737864 ) ) ;
#8639 = CARTESIAN_POINT ( 'NONE',  ( -3.916244202832140253, 2.131511515620587272, -4.187499998634405252 ) ) ;
#8640 = ORIENTED_EDGE ( 'NONE', *, *, #13761, .F. ) ;
#8641 = CARTESIAN_POINT ( 'NONE',  ( -7.500000000000005329, -3.640541674360518787, -0.7158139487964652048 ) ) ;
#8642 = EDGE_LOOP ( 'NONE', ( #8335, #1736, #7511, #4624 ) ) ;
#8643 = VERTEX_POINT ( 'NONE', #4592 ) ;
#8644 = CARTESIAN_POINT ( 'NONE',  ( -7.500000000000000888, -4.652405105468739421, -7.929127756970859586 ) ) ;
#8645 = AXIS2_PLACEMENT_3D ( 'NONE', #1066, #6002, #837 ) ;
#8646 = CARTESIAN_POINT ( 'NONE',  ( -4.458734125000000326, -23.00000000136559564, -1.846868145590735644 ) ) ;
#8647 = CARTESIAN_POINT ( 'NONE',  ( 7.894787914004607998, 1.231001383561881556E-13, -7.591390474663423760 ) ) ;
#8648 = AXIS2_PLACEMENT_3D ( 'NONE', #7260, #7333, #3766 ) ;
#8649 = EDGE_LOOP ( 'NONE', ( #15044, #4484, #270, #14984 ) ) ;
#8650 = DIRECTION ( 'NONE',  ( -0.5000000000000002220, 0.000000000000000000, 0.8660254037844383745 ) ) ;
#8651 = DIRECTION ( 'NONE',  ( 0.000000000000000000, 0.000000000000000000, 1.000000000000000000 ) ) ;
#8652 = CARTESIAN_POINT ( 'NONE',  ( 0.000000000000000000, 0.000000000000000000, -25.03750572909317285 ) ) ;
#8653 = DIRECTION ( 'NONE',  ( 0.000000000000000000, -1.000000000000000000, 0.000000000000000000 ) ) ;
#8654 = VECTOR ( 'NONE', #12635, 1000.000000000000000 ) ;
#8655 = CARTESIAN_POINT ( 'NONE',  ( -4.458734125000000326, -25.25000000136559564, -1.846868145590735644 ) ) ;
#8656 = CYLINDRICAL_SURFACE ( 'NONE', #1395, 9.999999999999994671 ) ;
#8657 = PLANE ( 'NONE',  #13592 ) ;
#8658 = CARTESIAN_POINT ( 'NONE',  ( -3.535533905932737309, -27.75000000273118772, -3.535533905932738197 ) ) ;
#8659 = AXIS2_PLACEMENT_3D ( 'NONE', #9016, #5128, #11262 ) ;
#8660 = CARTESIAN_POINT ( 'NONE',  ( 2.500000000000000000, 0.000000000000000000, 0.000000000000000000 ) ) ;
#8661 = CARTESIAN_POINT ( 'NONE',  ( 2.730187237215162345E-16, -30.18750000136559564, -4.458734124999999437 ) ) ;
#8662 = EDGE_CURVE ( 'NONE', #12101, #7457, #731, .T. ) ;
#8663 = ORIENTED_EDGE ( 'NONE', *, *, #867, .F. ) ;
#8664 = ORIENTED_EDGE ( 'NONE', *, *, #3327, .T. ) ;
#8665 = CARTESIAN_POINT ( 'NONE',  ( 1.734723475976807094E-15, 4.618802153517012954, -0.4999999999999995559 ) ) ;
#8666 = CIRCLE ( 'NONE', #1689, 25.00000000000000000 ) ;
#8667 = ORIENTED_EDGE ( 'NONE', *, *, #7538, .T. ) ;
#8668 = DIRECTION ( 'NONE',  ( -0.8660254037844410391, 0.4999999999999958367, -0.000000000000000000 ) ) ;
#8669 = AXIS2_PLACEMENT_3D ( 'NONE', #5921, #10844, #14556 ) ;
#8670 = CARTESIAN_POINT ( 'NONE',  ( 3.401574460001763445, -4.209348295687703079, -4.062499997268815832 ) ) ;
#8671 = CARTESIAN_POINT ( 'NONE',  ( 1.261996585732578113, -4.276409079477644148, -3.562499998634407916 ) ) ;
#8672 = PRODUCT_CONTEXT ( 'NONE', #723, 'mechanical' ) ;
#8673 = VECTOR ( 'NONE', #4970, 1000.000000000000000 ) ;
#8674 = CARTESIAN_POINT ( 'NONE',  ( -4.276409079477644148, -1.261996585732578335, -4.062499998634405252 ) ) ;
#8675 = CARTESIAN_POINT ( 'NONE',  ( -115.0000000000000142, -10.00000000000000888, -17.50000000000000000 ) ) ;
#8676 = EDGE_CURVE ( 'NONE', #6321, #14345, #2775, .T. ) ;
#8677 = DIRECTION ( 'NONE',  ( 0.4999999999999998335, -0.000000000000000000, 0.8660254037844387076 ) ) ;
#8679 = ADVANCED_FACE ( 'NONE', ( #10662 ), #9757, .T. ) ;
#8678 = ORIENTED_EDGE ( 'NONE', *, *, #11551, .F. ) ;
#8680 = VECTOR ( 'NONE', #2564, 1000.000000000000000 ) ;
#8681 = DIRECTION ( 'NONE',  ( 0.000000000000000000, 0.000000000000000000, 1.000000000000000000 ) ) ;
#8682 = ORIENTED_EDGE ( 'NONE', *, *, #15378, .F. ) ;
#8683 = FACE_OUTER_BOUND ( 'NONE', #7018, .T. ) ;
#8684 = EDGE_LOOP ( 'NONE', ( #14969, #4952, #3010, #583 ) ) ;
#8685 = ORIENTED_EDGE ( 'NONE', *, *, #5718, .T. ) ;
#8686 = CARTESIAN_POINT ( 'NONE',  ( -0.5093500532425060401, -4.799145180956616130, -4.874999998634406140 ) ) ;
#8687 = CARTESIAN_POINT ( 'NONE',  ( -3.401574460001765221, 4.209348295687701302, -4.562499997268816720 ) ) ;
#8688 = AXIS2_PLACEMENT_3D ( 'NONE', #9270, #4412, #9344 ) ;
#8689 = DIRECTION ( 'NONE',  ( -1.000000000000000000, -0.000000000000000000, -0.000000000000000000 ) ) ;
#8690 = DIRECTION ( 'NONE',  ( -0.000000000000000000, 1.000000000000000000, -0.000000000000000000 ) ) ;
#8691 = UNCERTAINTY_MEASURE_WITH_UNIT (LENGTH_MEASURE( 1.000000000000000082E-05 ), #11921, 'distance_accuracy_value', 'NONE');
#8692 = CARTESIAN_POINT ( 'NONE',  ( 2.071067811865476394, -27.31250000273118772, 5.000000000000000000 ) ) ;
#8693 = CARTESIAN_POINT ( 'NONE',  ( 4.391654775818395251, -2.390265326283149694, -3.999999997268816720 ) ) ;
#8694 = CARTESIAN_POINT ( 'NONE',  ( -3.535533905932737309, -24.62500000000000000, -3.535533905932738197 ) ) ;
#8695 = EDGE_CURVE ( 'NONE', #4042, #8451, #6415, .T. ) ;
#8696 = AXIS2_PLACEMENT_3D ( 'NONE', #12162, #1100, #2462 ) ;
#8697 = DIRECTION ( 'NONE',  ( -0.000000000000000000, 1.000000000000000000, -0.000000000000000000 ) ) ;
#8698 = CARTESIAN_POINT ( 'NONE',  ( -1.846868145590737420, -25.00000000136559564, 4.458734124999997661 ) ) ;
#8699 = ADVANCED_FACE ( 'NONE', ( #1923 ), #14298, .T. ) ;
#8700 = VERTEX_POINT ( 'NONE', #8170 ) ;
#8701 = CARTESIAN_POINT ( 'NONE',  ( -4.458734124999999437, -24.00000000136559564, -1.846868145590735644 ) ) ;
#8702 = CARTESIAN_POINT ( 'NONE',  ( 3.916244202832140253, -2.131511515620588160, -3.437499998634407916 ) ) ;
#8703 = FACE_OUTER_BOUND ( 'NONE', #5517, .T. ) ;
#8704 = ORIENTED_EDGE ( 'NONE', *, *, #7629, .F. ) ;
#8705 = ORIENTED_EDGE ( 'NONE', *, *, #4867, .T. ) ;
#8706 = VECTOR ( 'NONE', #584, 1000.000000000000000 ) ;
#8707 = DIRECTION ( 'NONE',  ( -0.4999999999999919509, 0.000000000000000000, -0.8660254037844432595 ) ) ;
#8708 = ORIENTED_EDGE ( 'NONE', *, *, #3445, .F. ) ;
#8709 = CARTESIAN_POINT ( 'NONE',  ( 4.458734124999999437, -21.75000000136559564, 1.846868145590737864 ) ) ;
#8710 = LINE ( 'NONE', #61, #7140 ) ;
#8711 = DIRECTION ( 'NONE',  ( -0.8660254037844387076, 0.000000000000000000, 0.4999999999999997224 ) ) ;
#8712 = VECTOR ( 'NONE', #5044, 1000.000000000000000 ) ;
#8713 = DIRECTION ( 'NONE',  ( 0.000000000000000000, 0.000000000000000000, 1.000000000000000000 ) ) ;
#8714 = DIRECTION ( 'NONE',  ( -0.000000000000000000, -1.000000000000000000, 0.000000000000000000 ) ) ;
#8715 = LINE ( 'NONE', #148, #8457 ) ;
#8716 = CARTESIAN_POINT ( 'NONE',  ( -5.381735091635034607, 0.5711823568785950878, -2.562500000000000888 ) ) ;
#8717 = CARTESIAN_POINT ( 'NONE',  ( -1.415196051561583790, 4.795541693661363958, -3.750000000000000000 ) ) ;
#8718 = EDGE_CURVE ( 'NONE', #3403, #14772, #5969, .T. ) ;
#8719 = FACE_OUTER_BOUND ( 'NONE', #14361, .T. ) ;
#8720 = CARTESIAN_POINT ( 'NONE',  ( -3.152801135295367096, -26.06250000136559564, -3.152801135295367541 ) ) ;
#8721 =( BOUNDED_SURFACE ( )  B_SPLINE_SURFACE ( 3, 2, ( 
 ( #11440, #15257, #6288 ),
 ( #10331, #12566, #1514 ),
 ( #314, #1422, #11364 ),
 ( #6604, #13866, #13775 ),
 ( #6452, #3855, #2631 ),
 ( #9041, #10085, #7582 ),
 ( #5225, #6369, #10161 ),
 ( #11519, #2799, #2711 ) ),
 .UNSPECIFIED., .F., .F., .F. ) 
 B_SPLINE_SURFACE_WITH_KNOTS ( ( 4, 2, 2, 4 ),
 ( 3, 3 ),
 ( 0.03861844051980971304, 0.04325213341840643266, 0.04556897986770479247, 0.04788582631700314535 ),
 ( 0.000000000000000000, 1.000000000000000000 ),
 .UNSPECIFIED. ) 
 GEOMETRIC_REPRESENTATION_ITEM ( )  RATIONAL_B_SPLINE_SURFACE ( (
 ( 1.000000000000000000, 0.8047781759831923454, 1.000000000000000000),
 ( 1.000000000000000000, 0.8123762462804495765, 1.000000000000000000),
 ( 1.000000000000000000, 0.8190659850617496573, 1.000000000000000000),
 ( 1.000000000000000000, 0.8191937571013253594, 1.000000000000000000),
 ( 1.000000000000000000, 0.8176092952781198742, 1.000000000000000000),
 ( 1.000000000000000000, 0.8122962088595745422, 1.000000000000000000),
 ( 1.000000000000000000, 0.8086311330828506172, 1.000000000000000000),
 ( 1.000000000000000000, 0.8047712282214323221, 1.000000000000000000) ) ) 
 REPRESENTATION_ITEM ( '' )  SURFACE ( )  );
#8722 = EDGE_CURVE ( 'NONE', #11884, #11709, #8562, .T. ) ;
#8723 = CARTESIAN_POINT ( 'NONE',  ( 0.5093500532425063732, 4.799145180956616130, -4.374999998634405252 ) ) ;
#8724 = ORIENTED_EDGE ( 'NONE', *, *, #6525, .F. ) ;
#8725 = CIRCLE ( 'NONE', #1742, 1.999999999999998224 ) ;
#8726 = CARTESIAN_POINT ( 'NONE',  ( -7.894787914004611551, -0.7661396099416333261, -7.591390474663429089 ) ) ;
#8727 = EDGE_LOOP ( 'NONE', ( #6944, #2012 ) ) ;
#8728 = VERTEX_POINT ( 'NONE', #3530 ) ;
#8729 = CARTESIAN_POINT ( 'NONE',  ( -4.000000000000000000, -2.472261339043343220, -3.687027428081192326 ) ) ;
#8730 = CARTESIAN_POINT ( 'NONE',  ( -8.190561711645485556E-16, -26.68750000136559564, 4.458734124999999437 ) ) ;
#8731 = DIRECTION ( 'NONE',  ( -0.000000000000000000, -1.000000000000000000, -0.000000000000000000 ) ) ;
#8732 = ORIENTED_EDGE ( 'NONE', *, *, #7686, .T. ) ;
#8733 = VECTOR ( 'NONE', #15639, 1000.000000000000000 ) ;
#8734 = FACE_OUTER_BOUND ( 'NONE', #12454, .T. ) ;
#8736 = CIRCLE ( 'NONE', #10793, 10.39117206796836079 ) ;
#8735 = DIRECTION ( 'NONE',  ( -0.000000000000000000, 1.000000000000000000, -0.000000000000000000 ) ) ;
#8737 = CARTESIAN_POINT ( 'NONE',  ( -91.33974596215558961, -105.7735026918962262, 7.500000000000001776 ) ) ;
#8738 = VECTOR ( 'NONE', #6662, 1000.000000000000000 ) ;
#8739 = CARTESIAN_POINT ( 'NONE',  ( -5.000000000000000888, -29.56250000000000355, -2.071067811865475949 ) ) ;
#8740 = CARTESIAN_POINT ( 'NONE',  ( 6.000000000000000000, -13.00000000000000178, 1.500000000000000000 ) ) ;
#8741 = CARTESIAN_POINT ( 'NONE',  ( 2.500000000000000000, -1.178949249685213863, 2.042000000000002924 ) ) ;
#8742 = CARTESIAN_POINT ( 'NONE',  ( -3.535533905932737309, -26.75000000273118772, -3.535533905932738197 ) ) ;
#8743 = EDGE_CURVE ( 'NONE', #3154, #14037, #3561, .T. ) ;
#8744 = DIRECTION ( 'NONE',  ( 0.000000000000000000, 1.000000000000000000, -1.471414886128461471E-15 ) ) ;
#8745 = AXIS2_PLACEMENT_3D ( 'NONE', #4025, #12500, #8893 ) ;
#8746 = CARTESIAN_POINT ( 'NONE',  ( 5.000000000000000000, -24.18750000273119127, 2.071067811865478614 ) ) ;
#8747 =( LENGTH_UNIT ( ) NAMED_UNIT ( * ) SI_UNIT ( .MILLI., .METRE. ) );
#8748 = ORIENTED_EDGE ( 'NONE', *, *, #7361, .T. ) ;
#8749 = FILL_AREA_STYLE_COLOUR ( '', #2681 ) ;
#8750 = ORIENTED_EDGE ( 'NONE', *, *, #6097, .T. ) ;
#8751 = CARTESIAN_POINT ( 'NONE',  ( 4.535975386569504053, 1.338596318647080397, -8.156249999317205734 ) ) ;
#8752 = AXIS2_PLACEMENT_3D ( 'NONE', #5134, #2611, #12386 ) ;
#8753 = VECTOR ( 'NONE', #9176, 1000.000000000000114 ) ;
#8754 = ORIENTED_EDGE ( 'NONE', *, *, #13922, .F. ) ;
#8755 = DIRECTION ( 'NONE',  ( -0.000000000000000000, -1.000000000000000000, -0.000000000000000000 ) ) ;
#8756 = CIRCLE ( 'NONE', #13114, 9.999999999999980460 ) ;
#8757 = EDGE_CURVE ( 'NONE', #3896, #1633, #861, .T. ) ;
#8758 = DIRECTION ( 'NONE',  ( 0.000000000000000000, 0.000000000000000000, 1.000000000000000000 ) ) ;
#8759 = CARTESIAN_POINT ( 'NONE',  ( 4.799145180956616130, -0.5093500532425063732, -4.374999998634405252 ) ) ;
#8760 = AXIS2_PLACEMENT_3D ( 'NONE', #10106, #13967, #5336 ) ;
#8761 = AXIS2_PLACEMENT_3D ( 'NONE', #12585, #2571, #13717 ) ;
#8762 = CARTESIAN_POINT ( 'NONE',  ( -3.916244202832140253, 2.131511515620587272, -6.187499998634407028 ) ) ;
#8763 = CARTESIAN_POINT ( 'NONE',  ( 4.203833317240879275, 1.627343821129582979, -3.597273115243889929 ) ) ;
#8764 = DIRECTION ( 'NONE',  ( 0.000000000000000000, 0.000000000000000000, 1.000000000000000000 ) ) ;
#8765 = VERTEX_POINT ( 'NONE', #9596 ) ;
#8766 = CARTESIAN_POINT ( 'NONE',  ( -7.500000000000005329, 4.330127018922194537, -7.422398894150031623 ) ) ;
#8767 = ORIENTED_EDGE ( 'NONE', *, *, #14160, .F. ) ;
#8768 = CARTESIAN_POINT ( 'NONE',  ( 5.000000000000004441, 6.350331166892669572E-15, -1.045263047592943417 ) ) ;
#8769 = CARTESIAN_POINT ( 'NONE',  ( 3.152801135295367541, -31.31250000136559564, -3.152801135295367541 ) ) ;
#8770 = ORIENTED_EDGE ( 'NONE', *, *, #8358, .F. ) ;
#8771 = CARTESIAN_POINT ( 'NONE',  ( -3.033343224707664820, 3.753672977998667726, -8.249999998634409692 ) ) ;
#8772 = CARTESIAN_POINT ( 'NONE',  ( -9.184850993605147944E-16, -27.25000000000000000, 5.000000000000000000 ) ) ;
#8773 = EDGE_CURVE ( 'NONE', #3387, #7945, #8404, .T. ) ;
#8774 = EDGE_CURVE ( 'NONE', #10093, #6661, #1105, .T. ) ;
#8775 = B_SPLINE_CURVE_WITH_KNOTS ( 'NONE', 3,
 ( #4278, #10423, #3952, #12667, #13800, #4116, #9064, #5420, #14141, #2737, #11622, #15358, #1535, #7693, #15279, #2822 ),
 .UNSPECIFIED., .F., .F.,
 ( 4, 2, 2, 2, 2, 2, 2, 4 ),
 ( 0.000000000000000000, 0.0003988081628697498124, 0.0007976163257394996249, 0.001196424488609249383, 0.001595232651478999250, 0.001994040814348749333, 0.002392848977218498766, 0.003190465302957996331 ),
 .UNSPECIFIED. ) ;
#8776 = CARTESIAN_POINT ( 'NONE',  ( -2.000000000000006661, 3.464101615137750834, 0.000000000000000000 ) ) ;
#8777 = CARTESIAN_POINT ( 'NONE',  ( 2.143131898507869826E-15, 50.00000000000000000, -64.85000000000002274 ) ) ;
#8778 = CARTESIAN_POINT ( 'NONE',  ( -3.535533905932738641, -30.50000000273118772, 3.535533905932737309 ) ) ;
#8779 = CARTESIAN_POINT ( 'NONE',  ( 4.391654775818395251, -2.390265326283149694, -1.999999997268814944 ) ) ;
#8780 = CARTESIAN_POINT ( 'NONE',  ( 35.00000000000000000, 40.00000000000000000, -8.572527594031472993E-15 ) ) ;
#8781 = CARTESIAN_POINT ( 'NONE',  ( -4.361069479627173173, 1.579581656101586296, -0.2612589832309742399 ) ) ;
#8782 = CARTESIAN_POINT ( 'NONE',  ( 3.152801135295366208, -25.81250000136559564, 3.152801135295367985 ) ) ;
#8783 = ORIENTED_EDGE ( 'NONE', *, *, #4602, .T. ) ;
#8784 = DIRECTION ( 'NONE',  ( -1.000000000000000000, 0.000000000000000000, 0.000000000000000000 ) ) ;
#8785 = CARTESIAN_POINT ( 'NONE',  ( 1.261996585732578113, -4.276409079477644148, -3.562499998634407916 ) ) ;
#8786 = CARTESIAN_POINT ( 'NONE',  ( 0.000000000000000000, 0.000000000000000000, -5.000000000000000000 ) ) ;
#8787 = ORIENTED_EDGE ( 'NONE', *, *, #22, .F. ) ;
#8788 = EDGE_LOOP ( 'NONE', ( #111, #7959 ) ) ;
#8789 = ORIENTED_EDGE ( 'NONE', *, *, #10275, .T. ) ;
#8790 = CARTESIAN_POINT ( 'NONE',  ( -1.846868145590734756, -22.37500000136559564, -4.458734125000000326 ) ) ;
#8791 = DIRECTION ( 'NONE',  ( 0.000000000000000000, -1.000000000000000000, 1.471414886128461471E-15 ) ) ;
#8792 = CARTESIAN_POINT ( 'NONE',  ( -2.071067811865478170, -27.43750000273119127, 5.000000000000000000 ) ) ;
#8793 = EDGE_CURVE ( 'NONE', #14864, #13611, #4833, .T. ) ;
#8794 = CARTESIAN_POINT ( 'NONE',  ( -0.6508621380849234361, -8.763657152406455708, -7.907633014911227498 ) ) ;
#8795 = FACE_OUTER_BOUND ( 'NONE', #14699, .T. ) ;
#8796 = LINE ( 'NONE', #4004, #759 ) ;
#8797 = CARTESIAN_POINT ( 'NONE',  ( 1.415196051561583790, -4.795541693661363958, -6.250000000000001776 ) ) ;
#8798 = CARTESIAN_POINT ( 'NONE',  ( -4.391654775818395251, 2.390265326283148806, -2.625000000000002220 ) ) ;
#8799 = DIRECTION ( 'NONE',  ( 0.000000000000000000, 0.000000000000000000, -1.000000000000000000 ) ) ;
#8800 = CARTESIAN_POINT ( 'NONE',  ( -3.152801135295367985, -25.81250000136559564, 3.152801135295367096 ) ) ;
#8801 = CARTESIAN_POINT ( 'NONE',  ( 3.916244202832140253, -2.131511515620588160, -0.6874999986344089153 ) ) ;
#8802 = EDGE_LOOP ( 'NONE', ( #6517, #5974 ) ) ;
#8803 = CARTESIAN_POINT ( 'NONE',  ( -7.914973979435151463, -3.817460047930451239, -7.907502498112421563 ) ) ;
#8804 = VERTEX_POINT ( 'NONE', #4751 ) ;
#8805 = ORIENTED_EDGE ( 'NONE', *, *, #9663, .T. ) ;
#8806 = FACE_OUTER_BOUND ( 'NONE', #12365, .T. ) ;
#8807 = CARTESIAN_POINT ( 'NONE',  ( 4.458734124999999437, -24.43750000136559564, 0.000000000000000000 ) ) ;
#8808 = DIRECTION ( 'NONE',  ( 0.000000000000000000, 1.000000000000000000, 0.000000000000000000 ) ) ;
#8809 = EDGE_LOOP ( 'NONE', ( #1117, #4402, #11901, #3438 ) ) ;
#8810 = DIRECTION ( 'NONE',  ( 0.000000000000000000, 0.000000000000000000, -1.000000000000000000 ) ) ;
#8811 = EDGE_CURVE ( 'NONE', #15000, #14496, #11202, .T. ) ;
#8812 = EDGE_CURVE ( 'NONE', #1457, #138, #13875, .T. ) ;
#8813 = ADVANCED_FACE ( 'NONE', ( #5071, #10166 ), #11522, .T. ) ;
#8814 = ADVANCED_FACE ( 'NONE', ( #3932 ), #10791, .F. ) ;
#8815 = FACE_OUTER_BOUND ( 'NONE', #1371, .T. ) ;
#8816 = CARTESIAN_POINT ( 'NONE',  ( 3.033343224707661712, -3.753672977998669502, -0.4999999986344072500 ) ) ;
#8817 = CARTESIAN_POINT ( 'NONE',  ( 1.111665111977238718, 4.326204543705408412, -0.3789984458506780451 ) ) ;
#8818 =( BOUNDED_CURVE ( )  B_SPLINE_CURVE ( 2, ( #15201, #1691, #14458, #10740, #961, #2086, #15760, #5886, #15445 ),
 .UNSPECIFIED., .F., .F. ) 
 B_SPLINE_CURVE_WITH_KNOTS ( ( 3, 2, 2, 2, 3 ),
 ( 0.9249999999999998224, 0.9374999999999997780, 0.9499999999999998446, 0.9624999999999999112, 0.9749999999999998668 ),
 .UNSPECIFIED. ) 
 CURVE ( )  GEOMETRIC_REPRESENTATION_ITEM ( )  RATIONAL_B_SPLINE_CURVE ( ( 1.000000000000001332, 0.9238795325112854062, 1.000000000000000000, 0.9238795325112867385, 1.000000000000000000, 0.9238795325112867385, 1.000000000000000000, 0.9238795325112874046, 0.9999999999999993339 ) ) 
 REPRESENTATION_ITEM ( '' )  );
#8819 = CARTESIAN_POINT ( 'NONE',  ( 5.000000000000000888, -31.93750000000000355, -2.071067811865475505 ) ) ;
#8820 = LINE ( 'NONE', #15932, #5474 ) ;
#8821 = DIRECTION ( 'NONE',  ( 0.000000000000000000, 0.000000000000000000, 1.000000000000000000 ) ) ;
#8822 = CARTESIAN_POINT ( 'NONE',  ( 5.000000000000000888, -29.06250000273118772, -2.071067811865475505 ) ) ;
#8823 = DIRECTION ( 'NONE',  ( -0.000000000000000000, -1.000000000000000000, -0.000000000000000000 ) ) ;
#8824 = CARTESIAN_POINT ( 'NONE',  ( -4.458734124999999437, -28.93750000136559564, -5.460374474430324690E-16 ) ) ;
#8825 = FACE_OUTER_BOUND ( 'NONE', #12173, .T. ) ;
#8826 = ORIENTED_EDGE ( 'NONE', *, *, #13280, .F. ) ;
#8827 = ORIENTED_EDGE ( 'NONE', *, *, #14085, .F. ) ;
#8828 = VERTEX_POINT ( 'NONE', #11291 ) ;
#8829 = CARTESIAN_POINT ( 'NONE',  ( 0.000000000000000000, -20.00000000000000000, 0.000000000000000000 ) ) ;
#8830 = ORIENTED_EDGE ( 'NONE', *, *, #8998, .F. ) ;
#8831 = CARTESIAN_POINT ( 'NONE',  ( -28.86751345948129455, -3.000000000000000000, 22.00000000000000711 ) ) ;
#8832 = EDGE_CURVE ( 'NONE', #9262, #10619, #4987, .T. ) ;
#8833 = CARTESIAN_POINT ( 'NONE',  ( 0.000000000000000000, 20.00000000000000000, 25.00000000000000000 ) ) ;
#8834 = CIRCLE ( 'NONE', #10638, 2.649999999999985700 ) ;
#8835 = DIRECTION ( 'NONE',  ( -6.123233995736766036E-17, -1.000000000000000000, -4.275831445896958607E-31 ) ) ;
#8836 = CARTESIAN_POINT ( 'NONE',  ( -2.131511515620587272, -3.916244202832140253, -6.937499998634407916 ) ) ;
#8837 = CYLINDRICAL_SURFACE ( 'NONE', #3548, 31.99999999999999289 ) ;
#8838 = DIRECTION ( 'NONE',  ( -0.000000000000000000, -1.000000000000000000, -0.000000000000000000 ) ) ;
#8839 = VERTEX_POINT ( 'NONE', #242 ) ;
#8840 = DIRECTION ( 'NONE',  ( 0.000000000000000000, 0.000000000000000000, 1.000000000000000000 ) ) ;
#8841 = B_SPLINE_CURVE_WITH_KNOTS ( 'NONE', 3,
 ( #2990, #1373, #5430, #12440, #11558, #9074 ),
 .UNSPECIFIED., .F., .F.,
 ( 4, 2, 4 ),
 ( 0.000000000000000000, 0.0004189869898914150835, 0.0008379739797828320100 ),
 .UNSPECIFIED. ) ;
#8842 = ORIENTED_EDGE ( 'NONE', *, *, #7794, .F. ) ;
#8843 = DIRECTION ( 'NONE',  ( 1.734723475976808080E-16, -1.000000000000000000, -2.407412430484045692E-31 ) ) ;
#8844 = DIRECTION ( 'NONE',  ( -0.000000000000000000, -1.000000000000000000, -0.000000000000000000 ) ) ;
#8845 = EDGE_LOOP ( 'NONE', ( #11934, #1215 ) ) ;
#8846 = CONTEXT_DEPENDENT_SHAPE_REPRESENTATION ( #2995, #43 ) ;
#8847 = CARTESIAN_POINT ( 'NONE',  ( -4.276409079477644148, -1.261996585732578335, -8.062499998634407916 ) ) ;
#8848 = CARTESIAN_POINT ( 'NONE',  ( 2.390265326283148806, 4.391654775818395251, -4.749999997268817609 ) ) ;
#8849 = AXIS2_PLACEMENT_3D ( 'NONE', #9214, #10658, #12907 ) ;
#8850 = FACE_OUTER_BOUND ( 'NONE', #11257, .T. ) ;
#8851 = CARTESIAN_POINT ( 'NONE',  ( -3.093157300003891663, -6.874418838041295388, -4.773877690725237500E-15 ) ) ;
#8852 = PRODUCT_DEFINITION_CONTEXT ( 'detailed design', #327, 'design' ) ;
#8853 = CARTESIAN_POINT ( 'NONE',  ( 14.41154273188009682, -35.00000000000000000, 60.96152422706633445 ) ) ;
#8854 = CARTESIAN_POINT ( 'NONE',  ( 4.795541693661363958, 1.415196051561583790, -3.874999997268816720 ) ) ;
#8855 = CARTESIAN_POINT ( 'NONE',  ( 0.5711823568785988625, 5.381735091635026613, -8.687499997268814056 ) ) ;
#8856 = DIRECTION ( 'NONE',  ( 0.000000000000000000, 0.000000000000000000, -1.000000000000000000 ) ) ;
#8857 = LINE ( 'NONE', #15156, #13022 ) ;
#8858 = ORIENTED_EDGE ( 'NONE', *, *, #12208, .F. ) ;
#8859 = FACE_OUTER_BOUND ( 'NONE', #11536, .T. ) ;
#8860 = CARTESIAN_POINT ( 'NONE',  ( 2.131511515620586383, 3.916244202832140253, -7.187499998634407916 ) ) ;
#8861 = DIRECTION ( 'NONE',  ( 0.000000000000000000, 0.000000000000000000, 1.000000000000000000 ) ) ;
#8862 = EDGE_CURVE ( 'NONE', #7310, #6759, #6456, .T. ) ;
#8863 = ORIENTED_EDGE ( 'NONE', *, *, #2752, .F. ) ;
#8864 = ORIENTED_EDGE ( 'NONE', *, *, #10715, .F. ) ;
#8865 = EDGE_CURVE ( 'NONE', #2621, #3171, #13356, .T. ) ;
#8866 = ORIENTED_EDGE ( 'NONE', *, *, #6987, .F. ) ;
#8867 = CARTESIAN_POINT ( 'NONE',  ( 4.769696007084728073, -13.00000000000000178, -1.500000000000000000 ) ) ;
#8868 = DIRECTION ( 'NONE',  ( 0.000000000000000000, 1.000000000000000000, 0.000000000000000000 ) ) ;
#8869 = CARTESIAN_POINT ( 'NONE',  ( 24.26932219902320043, 20.00000000000000000, 5.999999999999992895 ) ) ;
#8870 = VECTOR ( 'NONE', #3690, 1000.000000000000000 ) ;
#8871 = CARTESIAN_POINT ( 'NONE',  ( 0.2500000000000002220, 0.000000000000000000, 0.000000000000000000 ) ) ;
#8872 = CARTESIAN_POINT ( 'NONE',  ( -35.00000000000000000, 37.00000000000000000, 0.000000000000000000 ) ) ;
#8873 = CARTESIAN_POINT ( 'NONE',  ( 2.500000000000000000, -1.178949249685213863, 2.042000000000002924 ) ) ;
#8874 = CARTESIAN_POINT ( 'NONE',  ( 5.381735091635035495, -0.5711823568785978633, -4.062499999999999112 ) ) ;
#8875 = CARTESIAN_POINT ( 'NONE',  ( 3.535533905932738197, -29.87500000000000000, -3.535533905932738197 ) ) ;
#8876 = CARTESIAN_POINT ( 'NONE',  ( -39.99999999999999289, -11.00000000000000178, 2.500000000001739497 ) ) ;
#8877 = CARTESIAN_POINT ( 'NONE',  ( 3.152801135295366208, -24.56250000136559564, 3.152801135295367985 ) ) ;
#8878 = CARTESIAN_POINT ( 'NONE',  ( 4.799145180956616130, -0.5093500532425063732, -7.624999998634408804 ) ) ;
#8879 = EDGE_LOOP ( 'NONE', ( #2332, #9585, #9326, #696 ) ) ;
#8880 = DIRECTION ( 'NONE',  ( -1.000000000000000000, 0.000000000000000000, 0.000000000000000000 ) ) ;
#8881 = ADVANCED_FACE ( 'NONE', ( #7831 ), #14930, .F. ) ;
#8882 = ORIENTED_EDGE ( 'NONE', *, *, #5905, .F. ) ;
#8883 = VERTEX_POINT ( 'NONE', #12727 ) ;
#8884 = ADVANCED_FACE ( 'NONE', ( #8719 ), #13625, .T. ) ;
#8885 = PRODUCT_RELATED_PRODUCT_CATEGORY ( 'part', '', ( #4208 ) ) ;
#8886 =( REPRESENTATION_RELATIONSHIP ('NONE','NONE', #4176, #279 ) REPRESENTATION_RELATIONSHIP_WITH_TRANSFORMATION ( #12764 )SHAPE_REPRESENTATION_RELATIONSHIP( ) );
#8887 = CARTESIAN_POINT ( 'NONE',  ( 3.152801135295367541, -22.31250000136559564, -3.152801135295367541 ) ) ;
#8888 = LINE ( 'NONE', #13790, #1704 ) ;
#8889 = VERTEX_POINT ( 'NONE', #8876 ) ;
#8890 = MECHANICAL_DESIGN_GEOMETRIC_PRESENTATION_REPRESENTATION (  '', ( #8632 ), #12213 ) ;
#8891 = CARTESIAN_POINT ( 'NONE',  ( 0.6640947660595348800, -4.471078309994175548, -3.602146406945708090 ) ) ;
#8892 = CARTESIAN_POINT ( 'NONE',  ( 7.500000000000000000, -4.730916290271727220, -7.493595886788497751 ) ) ;
#8893 = DIRECTION ( 'NONE',  ( 0.000000000000000000, 0.000000000000000000, 1.000000000000000000 ) ) ;
#8894 = LINE ( 'NONE', #13796, #15576 ) ;
#8895 = CARTESIAN_POINT ( 'NONE',  ( -3.535533905932738641, -29.37500000000000355, 3.535533905932737309 ) ) ;
#8896 = FACE_OUTER_BOUND ( 'NONE', #5366, .T. ) ;
#8897 = PLANE ( 'NONE',  #4582 ) ;
#8898 = CARTESIAN_POINT ( 'NONE',  ( 3.061616997868383141E-16, -27.87500000273118772, -5.000000000000000000 ) ) ;
#8899 = CARTESIAN_POINT ( 'NONE',  ( 0.000000000000000000, 0.000000000000000000, -25.03750572909317285 ) ) ;
#8900 =( GEOMETRIC_REPRESENTATION_CONTEXT ( 3 ) GLOBAL_UNCERTAINTY_ASSIGNED_CONTEXT ( ( #14825 ) ) GLOBAL_UNIT_ASSIGNED_CONTEXT ( ( #4462, #10767, #10535 ) ) REPRESENTATION_CONTEXT ( 'NONE', 'WORKASPACE' ) );
#8901 = CARTESIAN_POINT ( 'NONE',  ( -3.152801135295367985, -29.81250000136559208, 3.152801135295367096 ) ) ;
#8902 = EDGE_CURVE ( 'NONE', #6090, #869, #4863, .T. ) ;
#8903 =( NAMED_UNIT ( * ) SI_UNIT ( $, .STERADIAN. ) SOLID_ANGLE_UNIT ( ) );
#8904 = ORIENTED_EDGE ( 'NONE', *, *, #4007, .T. ) ;
#8905 = PRODUCT_DEFINITION ( 'UNKNOWN', '', #13325, #11421 ) ;
#8906 = ORIENTED_EDGE ( 'NONE', *, *, #1811, .T. ) ;
#8907 = EDGE_CURVE ( 'NONE', #6536, #7472, #5230, .T. ) ;
#8908 = CIRCLE ( 'NONE', #11716, 4.000000000000000000 ) ;
#8909 = AXIS2_PLACEMENT_3D ( 'NONE', #5005, #9934, #14872 ) ;
#8910 = ORIENTED_EDGE ( 'NONE', *, *, #2948, .F. ) ;
#8911 = CARTESIAN_POINT ( 'NONE',  ( -44.43024643319441225, -4.732646668676770751, 20.01350297727719507 ) ) ;
#8912 = ORIENTED_EDGE ( 'NONE', *, *, #6122, .F. ) ;
#8913 = PLANE ( 'NONE',  #1202 ) ;
#8914 = PRESENTATION_LAYER_ASSIGNMENT (  '', '', ( #2178 ) ) ;
#8915 = CARTESIAN_POINT ( 'NONE',  ( -2.071067811865477726, -31.68750000000000000, -4.999999999999996447 ) ) ;
#8916 = AXIS2_PLACEMENT_3D ( 'NONE', #9274, #855, #626 ) ;
#8917 = CARTESIAN_POINT ( 'NONE',  ( -43.99999999999978684, -11.00000000000000178, -1.500000000000000666 ) ) ;
#8918 = CARTESIAN_POINT ( 'NONE',  ( 5.000000000000000000, -22.00000000000000000, 0.000000000000000000 ) ) ;
#8919 = CARTESIAN_POINT ( 'NONE',  ( 2.131511515620586383, 3.916244202832140253, -4.437499998634405252 ) ) ;
#8920 = LINE ( 'NONE', #7631, #6107 ) ;
#8921 = ORIENTED_EDGE ( 'NONE', *, *, #12035, .T. ) ;
#8922 = DIRECTION ( 'NONE',  ( 1.000000000000000000, 0.000000000000000000, 0.000000000000000000 ) ) ;
#8923 = EDGE_CURVE ( 'NONE', #6, #11302, #10289, .T. ) ;
#8924 = CIRCLE ( 'NONE', #14324, 2.649999999999985700 ) ;
#8925 = ORIENTED_EDGE ( 'NONE', *, *, #7920, .F. ) ;
#8926 = CARTESIAN_POINT ( 'NONE',  ( -0.5711823568785977523, -5.381735091635034607, -7.312500000000006217 ) ) ;
#8927 = CARTESIAN_POINT ( 'NONE',  ( -36.99999999999999289, -11.00000000000000178, -3.999999999999170885 ) ) ;
#8928 = AXIS2_PLACEMENT_3D ( 'NONE', #3339, #9557, #9708 ) ;
#8929 = EDGE_LOOP ( 'NONE', ( #6533, #9658, #4636 ) ) ;
#8930 = CARTESIAN_POINT ( 'NONE',  ( 4.276409079477644148, 1.261996585732577891, -6.562499998634407028 ) ) ;
#8931 = CIRCLE ( 'NONE', #4528, 2.000000000000000888 ) ;
#8932 = CARTESIAN_POINT ( 'NONE',  ( 5.200000000000002842, 0.000000000000000000, 0.000000000000000000 ) ) ;
#8933 = DIRECTION ( 'NONE',  ( 0.000000000000000000, 0.000000000000000000, -1.000000000000000000 ) ) ;
#8934 = AXIS2_PLACEMENT_3D ( 'NONE', #6644, #12514, #12600 ) ;
#8935 = CARTESIAN_POINT ( 'NONE',  ( 2.071067811865468844, -26.93750000273118772, -5.000000000000007994 ) ) ;
#8936 = AXIS2_PLACEMENT_3D ( 'NONE', #13960, #6540, #4187 ) ;
#8937 = CARTESIAN_POINT ( 'NONE',  ( 4.795541693661363958, 1.415196051561583790, -5.874999997268814944 ) ) ;
#8938 = DIRECTION ( 'NONE',  ( 1.000000000000000000, 1.541976423090495140E-16, -0.000000000000000000 ) ) ;
#8939 = CARTESIAN_POINT ( 'NONE',  ( -1.036170633859778700, 4.395255856367823455, -0.3471699856533662087 ) ) ;
#8940 = CARTESIAN_POINT ( 'NONE',  ( 35.00000000000000000, 37.00000000000000000, -8.572527594031472993E-15 ) ) ;
#8941 = ORIENTED_EDGE ( 'NONE', *, *, #8575, .T. ) ;
#8942 = DIRECTION ( 'NONE',  ( 0.5000000000000002220, 0.000000000000000000, -0.8660254037844384856 ) ) ;
#8943 = CARTESIAN_POINT ( 'NONE',  ( -28.86751345948112402, 0.000000000000000000, 18.00000000000026645 ) ) ;
#8944 = DIRECTION ( 'NONE',  ( 1.000000000000000000, 0.000000000000000000, 0.000000000000000000 ) ) ;
#8945 = ORIENTED_EDGE ( 'NONE', *, *, #15905, .F. ) ;
#8946 = ORIENTED_EDGE ( 'NONE', *, *, #13380, .F. ) ;
#8947 = ORIENTED_EDGE ( 'NONE', *, *, #14917, .T. ) ;
#8948 = CARTESIAN_POINT ( 'NONE',  ( -0.6666666666666666297, -4.233901974057276973, -3.300726591567087365 ) ) ;
#8949 = FACE_OUTER_BOUND ( 'NONE', #12491, .T. ) ;
#8950 = AXIS2_PLACEMENT_3D ( 'NONE', #10343, #15433, #6710 ) ;
#8951 = DIRECTION ( 'NONE',  ( 0.000000000000000000, 1.000000000000000000, 0.000000000000000000 ) ) ;
#8952 = CIRCLE ( 'NONE', #15666, 10.00000000000000711 ) ;
#8953 = ADVANCED_FACE ( 'NONE', ( #15261 ), #8995, .F. ) ;
#8954 = DIRECTION ( 'NONE',  ( 0.000000000000000000, 0.000000000000000000, 1.000000000000000000 ) ) ;
#8956 = PLANE ( 'NONE',  #13998 ) ;
#8955 = AXIS2_PLACEMENT_3D ( 'NONE', #12687, #13578, #6251 ) ;
#8957 = PLANE ( 'NONE',  #7459 ) ;
#8958 = CARTESIAN_POINT ( 'NONE',  ( -4.795541693661363958, -1.415196051561583790, -3.499999999999999556 ) ) ;
#8959 = DIRECTION ( 'NONE',  ( -0.000000000000000000, 1.000000000000000000, -0.000000000000000000 ) ) ;
#8960 = CARTESIAN_POINT ( 'NONE',  ( -1.274258131565027874, -3.883108878240886241, -3.220599429844051009 ) ) ;
#8961 = CARTESIAN_POINT ( 'NONE',  ( 1.846868145590736310, -22.62500000136559564, 4.458734124999999437 ) ) ;
#8962 = AXIS2_PLACEMENT_3D ( 'NONE', #3724, #14431, #13192 ) ;
#8963 = CARTESIAN_POINT ( 'NONE',  ( -2.131511515620587272, -3.916244202832140253, -7.937499998634408804 ) ) ;
#8964 = ORIENTED_EDGE ( 'NONE', *, *, #5448, .T. ) ;
#8965 = CARTESIAN_POINT ( 'NONE',  ( 6.874999999999999112, 4.690970937165705124, -7.298562697733105509 ) ) ;
#8966 = EDGE_LOOP ( 'NONE', ( #10172, #3956, #2108, #11233, #12060, #4481 ) ) ;
#8967 = VERTEX_POINT ( 'NONE', #15422 ) ;
#8968 = CARTESIAN_POINT ( 'NONE',  ( 2.730187237215162345E-16, -31.43750000136559564, -4.458734124999999437 ) ) ;
#8969 = FACE_OUTER_BOUND ( 'NONE', #8879, .T. ) ;
#8970 = AXIS2_PLACEMENT_3D ( 'NONE', #13504, #11909, #1012 ) ;
#8971 = ORIENTED_EDGE ( 'NONE', *, *, #10175, .F. ) ;
#8972 = CYLINDRICAL_SURFACE ( 'NONE', #644, 2.499999999999998668 ) ;
#8973 = PRODUCT_DEFINITION_FORMATION_WITH_SPECIFIED_SOURCE ( 'ANY', '', #6036, .NOT_KNOWN. ) ;
#8974 = DIRECTION ( 'NONE',  ( 1.114413700119375779E-16, 0.000000000000000000, -1.000000000000000000 ) ) ;
#8975 = EDGE_CURVE ( 'NONE', #4620, #12657, #4695, .T. ) ;
#8976 = CARTESIAN_POINT ( 'NONE',  ( -4.276409079477644148, -1.261996585732578335, -1.812499998634406584 ) ) ;
#8977 = DIRECTION ( 'NONE',  ( -0.000000000000000000, -1.000000000000000000, -0.000000000000000000 ) ) ;
#8978 = ADVANCED_FACE ( 'NONE', ( #5709 ), #2508, .T. ) ;
#8979 = CARTESIAN_POINT ( 'NONE',  ( 2.071067811865475505, -29.81249999999999645, -5.000000000000000888 ) ) ;
#8980 = CARTESIAN_POINT ( 'NONE',  ( -1.747541505913277282, 3.837784562140256650, -3.503702292528906526 ) ) ;
#8981 = CIRCLE ( 'NONE', #15946, 5.384454397937118664 ) ;
#8982 = DIRECTION ( 'NONE',  ( 1.000000000000000000, 0.000000000000000000, 0.000000000000000000 ) ) ;
#8983 = CARTESIAN_POINT ( 'NONE',  ( -2.071067811865475061, -22.81250000273118417, -5.000000000000000888 ) ) ;
#8984 = CARTESIAN_POINT ( 'NONE',  ( 0.000000000000000000, 0.000000000000000000, -0.5776712190230133270 ) ) ;
#8985 = CARTESIAN_POINT ( 'NONE',  ( 3.152801135295367541, -28.31250000136559564, -3.152801135295367541 ) ) ;
#8986 = APPLICATION_CONTEXT ( 'automotive_design' ) ;
#8987 = CARTESIAN_POINT ( 'NONE',  ( 10.00000000000098765, -13.00000000000000178, 14.82050807568871065 ) ) ;
#8988 = ORIENTED_EDGE ( 'NONE', *, *, #4725, .F. ) ;
#8989 = ORIENTED_EDGE ( 'NONE', *, *, #15462, .F. ) ;
#8990 = AXIS2_PLACEMENT_3D ( 'NONE', #303, #12785, #8784 ) ;
#8991 = ORIENTED_EDGE ( 'NONE', *, *, #10294, .T. ) ;
#8992 = DIRECTION ( 'NONE',  ( 0.000000000000000000, 0.000000000000000000, 1.000000000000000000 ) ) ;
#8993 = ORIENTED_EDGE ( 'NONE', *, *, #14598, .T. ) ;
#8994 = CYLINDRICAL_SURFACE ( 'NONE', #4315, 4.999999999999997335 ) ;
#8995 = CONICAL_SURFACE ( 'NONE', #15182, 2.041999999999999815, 1.047197551196591858 ) ;
#8996 = EDGE_CURVE ( 'NONE', #15957, #2273, #6149, .T. ) ;
#8997 = CARTESIAN_POINT ( 'NONE',  ( 16.49999999999956657, -8.782289339527253835E-13, -13.00000000000000000 ) ) ;
#8998 = EDGE_CURVE ( 'NONE', #15784, #15426, #3306, .T. ) ;
#8999 = CARTESIAN_POINT ( 'NONE',  ( 4.458734124999999437, -30.75000000136559564, 1.846868145590737864 ) ) ;
#9000 = AXIS2_PLACEMENT_3D ( 'NONE', #11660, #4235, #2051 ) ;
#9001 = CARTESIAN_POINT ( 'NONE',  ( -4.391654775818395251, 2.390265326283148806, -5.625000000000001776 ) ) ;
#9002 = CARTESIAN_POINT ( 'NONE',  ( 2.131511515620586383, 3.916244202832140253, -6.437499998634407028 ) ) ;
#9003 = DIRECTION ( 'NONE',  ( 0.000000000000000000, 0.000000000000000000, 1.000000000000000000 ) ) ;
#9004 = AXIS2_PLACEMENT_3D ( 'NONE', #9579, #8545, #14510 ) ;
#9005 = VERTEX_POINT ( 'NONE', #15577 ) ;
#9006 = CARTESIAN_POINT ( 'NONE',  ( 2.875844205641825191, -3.000000000000000000, -48.98110827882413787 ) ) ;
#9007 = PRESENTATION_LAYER_ASSIGNMENT (  '', '', ( #7720 ) ) ;
#9008 = FILL_AREA_STYLE ('',( #5120 ) ) ;
#9009 = ORIENTED_EDGE ( 'NONE', *, *, #223, .F. ) ;
#9010 = CARTESIAN_POINT ( 'NONE',  ( 17.00000000000000000, 2.516649172247811061E-16, -2.055000000000000160 ) ) ;
#9011 = CARTESIAN_POINT ( 'NONE',  ( 7.347880794884118356E-15, 40.00000000000000000, 60.00000000000000000 ) ) ;
#9012 = CIRCLE ( 'NONE', #14950, 2.649999999999992806 ) ;
#9013 = CIRCLE ( 'NONE', #15726, 4.000000000000000000 ) ;
#9014 = ORIENTED_EDGE ( 'NONE', *, *, #12842, .T. ) ;
#9015 = CARTESIAN_POINT ( 'NONE',  ( 2.131511515620586383, 3.916244202832140253, -5.437499998634406140 ) ) ;
#9016 = CARTESIAN_POINT ( 'NONE',  ( -115.0000000000000142, -10.00000000000000888, 17.50000000000000000 ) ) ;
#9017 = EDGE_CURVE ( 'NONE', #3976, #12516, #9430, .T. ) ;
#9018 = AXIS2_PLACEMENT_3D ( 'NONE', #10163, #6370, #6453 ) ;
#9019 = VECTOR ( 'NONE', #9212, 1000.000000000000000 ) ;
#9020 = EDGE_CURVE ( 'NONE', #7038, #12621, #5370, .T. ) ;
#9021 = CARTESIAN_POINT ( 'NONE',  ( 4.795541693661363958, 1.415196051561583790, -3.469446951953614189E-15 ) ) ;
#9022 = CARTESIAN_POINT ( 'NONE',  ( -0.5984201754795709371, -8.314755988442765755, -0.7022220667781371439 ) ) ;
#9023 = UNCERTAINTY_MEASURE_WITH_UNIT (LENGTH_MEASURE( 1.000000000000000082E-05 ), #15383, 'distance_accuracy_value', 'NONE');
#9024 = CARTESIAN_POINT ( 'NONE',  ( -0.5711823568785978633, -5.381735091635035495, -3.187499997268817609 ) ) ;
#9025 = DIRECTION ( 'NONE',  ( 0.000000000000000000, 1.000000000000000000, 0.000000000000000000 ) ) ;
#9026 = CARTESIAN_POINT ( 'NONE',  ( 19.99999999999956657, -8.786575603324269439E-13, -13.00000000000000000 ) ) ;
#9027 = DIRECTION ( 'NONE',  ( 0.000000000000000000, 0.000000000000000000, 1.000000000000000000 ) ) ;
#9028 = ORIENTED_EDGE ( 'NONE', *, *, #5503, .F. ) ;
#9029 = CARTESIAN_POINT ( 'NONE',  ( -44.99999999999999289, -11.00000000000000178, 4.000000000000831335 ) ) ;
#9030 = CARTESIAN_POINT ( 'NONE',  ( 7.500000000000000000, 4.330127018922190096, -7.422398894150031623 ) ) ;
#9031 = CARTESIAN_POINT ( 'NONE',  ( -60.00000000000000000, -5.000000000000000000, 17.99999999999999289 ) ) ;
#9032 = ORIENTED_EDGE ( 'NONE', *, *, #4051, .F. ) ;
#9033 = EDGE_LOOP ( 'NONE', ( #3293, #10984, #5257, #1350 ) ) ;
#9034 = ORIENTED_EDGE ( 'NONE', *, *, #6721, .T. ) ;
#9035 = VECTOR ( 'NONE', #7894, 1000.000000000000000 ) ;
#9036 = CARTESIAN_POINT ( 'NONE',  ( -1.305263714129176078, 8.377797850839289850, -7.792447862505333056 ) ) ;
#9037 = DIRECTION ( 'NONE',  ( -0.5000000000000051070, 1.060575238724903217E-16, -0.8660254037844355990 ) ) ;
#9038 = CARTESIAN_POINT ( 'NONE',  ( 10.00000000000098765, -20.00000000000000000, 14.82050807568871065 ) ) ;
#9039 = EDGE_CURVE ( 'NONE', #5622, #3351, #7625, .T. ) ;
#9040 = CYLINDRICAL_SURFACE ( 'NONE', #3282, 2.649999999999999467 ) ;
#9041 = CARTESIAN_POINT ( 'NONE',  ( -1.013163106017127779, -8.075304045852414347, -7.231838333420567366 ) ) ;
#9042 = DIRECTION ( 'NONE',  ( -1.000000000000000000, 6.938893903907228378E-16, 0.000000000000000000 ) ) ;
#9043 = CARTESIAN_POINT ( 'NONE',  ( -0.5711823568785978633, -5.381735091635035495, -7.312500000000004441 ) ) ;
#9044 = CARTESIAN_POINT ( 'NONE',  ( -17.99999999999979394, -9.000000000000001776, 3.499999999999998668 ) ) ;
#9045 = CARTESIAN_POINT ( 'NONE',  ( -1.390230914382372118, -4.043987460488664532, -3.502507215260523665 ) ) ;
#9046 = CARTESIAN_POINT ( 'NONE',  ( -1.846868145590737420, -24.75000000136559564, 4.458734124999999437 ) ) ;
#9047 = CARTESIAN_POINT ( 'NONE',  ( 2.131511515620586383, 3.916244202832140253, -6.437499998634407028 ) ) ;
#9048 = VERTEX_POINT ( 'NONE', #4419 ) ;
#9049 = CARTESIAN_POINT ( 'NONE',  ( 7.500000000000009770, -4.330127018922195425, -7.564338275809340040 ) ) ;
#9050 = VERTEX_POINT ( 'NONE', #12968 ) ;
#9051 = ORIENTED_EDGE ( 'NONE', *, *, #15927, .F. ) ;
#9052 = EDGE_LOOP ( 'NONE', ( #7783, #12254, #6339 ) ) ;
#9053 = CARTESIAN_POINT ( 'NONE',  ( 4.458734124999999437, -29.68750000136559208, 0.000000000000000000 ) ) ;
#9054 = ADVANCED_FACE ( 'NONE', ( #5398 ), #4344, .T. ) ;
#9055 = CARTESIAN_POINT ( 'NONE',  ( -39.99999999999999289, -11.00000000000000178, 8.300651832549021947E-13 ) ) ;
#9056 = EDGE_LOOP ( 'NONE', ( #9339, #7001 ) ) ;
#9057 = CARTESIAN_POINT ( 'NONE',  ( 4.141042297810615835, -2.227970268150433863, -3.687027686973623819 ) ) ;
#9058 =( BOUNDED_CURVE ( )  B_SPLINE_CURVE ( 3, ( #5795, #10731, #4742, #2315 ),
 .UNSPECIFIED., .F., .F. ) 
 B_SPLINE_CURVE_WITH_KNOTS ( ( 4, 4 ),
 ( 3.141592653589793116, 4.712388980384689674 ),
 .UNSPECIFIED. ) 
 CURVE ( )  GEOMETRIC_REPRESENTATION_ITEM ( )  RATIONAL_B_SPLINE_CURVE ( ( 1.000000000000000000, 0.8047378541243649375, 0.8047378541243649375, 1.000000000000000000 ) ) 
 REPRESENTATION_ITEM ( '' )  );
#9059 = DIRECTION ( 'NONE',  ( 0.000000000000000000, 0.5000000000000011102, 0.8660254037844380415 ) ) ;
#9060 = CARTESIAN_POINT ( 'NONE',  ( -0.5093500532425060401, -4.799145180956616130, -1.624999998634406362 ) ) ;
#9061 = CARTESIAN_POINT ( 'NONE',  ( -21.01110699893041911, -3.000000000000000000, -36.39230484541334221 ) ) ;
#9062 = CARTESIAN_POINT ( 'NONE',  ( -5.000000000000000888, -31.56249999999999645, -2.071067811865475949 ) ) ;
#9063 = CARTESIAN_POINT ( 'NONE',  ( -3.916244202832140253, 2.131511515620587272, -4.937499998634406140 ) ) ;
#9064 = CARTESIAN_POINT ( 'NONE',  ( -44.15480264658854992, -3.253774389711709958, -21.01641944516413574 ) ) ;
#9065 = DIRECTION ( 'NONE',  ( -1.000000000000000000, -0.000000000000000000, -0.000000000000000000 ) ) ;
#9066 = CARTESIAN_POINT ( 'NONE',  ( -5.000000000000000888, -24.68750000273118772, -2.071067811865475949 ) ) ;
#9067 = CARTESIAN_POINT ( 'NONE',  ( 0.000000000000000000, 0.000000000000000000, -0.2800830152838844622 ) ) ;
#9068 = CARTESIAN_POINT ( 'NONE',  ( -4.458734124999999437, -28.00000000136559564, -1.846868145590735644 ) ) ;
#9069 = ADVANCED_FACE ( 'NONE', ( #10335 ), #15340, .T. ) ;
#9070 = ORIENTED_EDGE ( 'NONE', *, *, #15170, .T. ) ;
#9071 = VERTEX_POINT ( 'NONE', #7993 ) ;
#9073 = ORIENTED_EDGE ( 'NONE', *, *, #1875, .F. ) ;
#9072 = ADVANCED_FACE ( 'NONE', ( #1903 ), #5113, .T. ) ;
#9074 = CARTESIAN_POINT ( 'NONE',  ( 7.922281120364393914, 4.573931137438269623, -8.047472243342932430 ) ) ;
#9075 = EDGE_CURVE ( 'NONE', #7770, #12513, #5635, .T. ) ;
#9076 = VERTEX_POINT ( 'NONE', #9353 ) ;
#9077 = DIRECTION ( 'NONE',  ( -0.000000000000000000, -1.000000000000000000, -0.000000000000000000 ) ) ;
#9078 = CARTESIAN_POINT ( 'NONE',  ( 0.000000000000000000, -20.00000000000000000, 0.000000000000000000 ) ) ;
#9079 = LINE ( 'NONE', #13820, #12863 ) ;
#9080 = DIRECTION ( 'NONE',  ( -0.000000000000000000, -1.000000000000000000, -0.000000000000000000 ) ) ;
#9081 = ITEM_DEFINED_TRANSFORMATION ( 'NONE', 'NONE', #2692,  #3223 ) ;
#9082 = DIRECTION ( 'NONE',  ( 0.000000000000000000, 1.000000000000000000, 0.000000000000000000 ) ) ;
#9083 = CARTESIAN_POINT ( 'NONE',  ( 3.033343224707661712, -3.753672977998669946, 0.2500000013655933606 ) ) ;
#9084 = EDGE_LOOP ( 'NONE', ( #13709, #14657, #15858, #4039, #12773 ) ) ;
#9085 = ADVANCED_BREP_SHAPE_REPRESENTATION ( '', ( #13909, #3223 ), #1673 ) ;
#9086 = EDGE_LOOP ( 'NONE', ( #6356, #5520, #11999, #1429 ) ) ;
#9087 = CARTESIAN_POINT ( 'NONE',  ( -28.86751345948130165, 0.000000000000000000, 18.00000000000000355 ) ) ;
#9088 = DIRECTION ( 'NONE',  ( 0.000000000000000000, 0.000000000000000000, 1.000000000000000000 ) ) ;
#9089 = ADVANCED_FACE ( 'NONE', ( #3201 ), #5950, .F. ) ;
#9090 = PRODUCT_RELATED_PRODUCT_CATEGORY ( 'part', '', ( #8362 ) ) ;
#9091 = VERTEX_POINT ( 'NONE', #2140 ) ;
#9092 = CARTESIAN_POINT ( 'NONE',  ( 19.99999999999956657, -8.786575603324269439E-13, 1.500000000000000000 ) ) ;
#9093 = CARTESIAN_POINT ( 'NONE',  ( 35.00000000000000000, 37.00000000000000000, -8.572527594031472993E-15 ) ) ;
#9094 = CARTESIAN_POINT ( 'NONE',  ( 0.000000000000000000, 50.00000000000000000, -75.00000000000004263 ) ) ;
#9095 = CARTESIAN_POINT ( 'NONE',  ( 4.209348295687701302, 3.401574460001765665, -8.812499997268814056 ) ) ;
#9096 = CARTESIAN_POINT ( 'NONE',  ( -3.535533905932738641, -23.37500000000000000, 3.535533905932737309 ) ) ;
#9097 = FACE_OUTER_BOUND ( 'NONE', #7161, .T. ) ;
#9098 = CARTESIAN_POINT ( 'NONE',  ( 2.730187237215162345E-16, -22.43750000136559564, -4.458734124999999437 ) ) ;
#9099 = ORIENTED_EDGE ( 'NONE', *, *, #3146, .F. ) ;
#9100 = DIRECTION ( 'NONE',  ( 0.000000000000000000, 1.000000000000000000, 0.000000000000000000 ) ) ;
#9101 = FACE_OUTER_BOUND ( 'NONE', #9084, .T. ) ;
#9102 = CARTESIAN_POINT ( 'NONE',  ( 6.288404560131952259, 5.029641972278930062, -0.4504974108211944883 ) ) ;
#9103 = EDGE_CURVE ( 'NONE', #13770, #14954, #8028, .T. ) ;
#9104 = VERTEX_POINT ( 'NONE', #3507 ) ;
#9105 = DIRECTION ( 'NONE',  ( 0.5000000000000002220, 2.602085213965209853E-15, -0.8660254037844383745 ) ) ;
#9106 = ORIENTED_EDGE ( 'NONE', *, *, #11651, .F. ) ;
#9107 = EDGE_CURVE ( 'NONE', #5402, #2543, #8736, .T. ) ;
#9108 = EDGE_CURVE ( 'NONE', #3157, #3489, #3816, .T. ) ;
#9109 = ORIENTED_EDGE ( 'NONE', *, *, #7626, .T. ) ;
#9110 = DIRECTION ( 'NONE',  ( 0.000000000000000000, 0.000000000000000000, 1.000000000000000000 ) ) ;
#9111 = DIRECTION ( 'NONE',  ( -0.000000000000000000, -1.000000000000000000, -0.000000000000000000 ) ) ;
#9112 = DIRECTION ( 'NONE',  ( 0.000000000000000000, 0.000000000000000000, 1.000000000000000000 ) ) ;
#9113 = MANIFOLD_SOLID_BREP ( 'Boss-Extrude1', #13832 ) ;
#9114 = LINE ( 'NONE', #12801, #1982 ) ;
#9115 = CARTESIAN_POINT ( 'NONE',  ( 5.000000000000000888, 4.250000000000000000, 0.000000000000000000 ) ) ;
#9116 = DIRECTION ( 'NONE',  ( 0.000000000000000000, 0.000000000000000000, 1.000000000000000000 ) ) ;
#9117 = VECTOR ( 'NONE', #7126, 999.9999999999998863 ) ;
#9118 = CARTESIAN_POINT ( 'NONE',  ( -3.401574460001764777, 4.209348295687701302, -3.687500000000000444 ) ) ;
#9119 = FACE_OUTER_BOUND ( 'NONE', #619, .T. ) ;
#9120 = DIRECTION ( 'NONE',  ( 0.000000000000000000, 0.000000000000000000, 1.000000000000000000 ) ) ;
#9121 = CARTESIAN_POINT ( 'NONE',  ( 4.458734125000000326, -24.37500000136559564, -1.846868145590734978 ) ) ;
#9122 = CARTESIAN_POINT ( 'NONE',  ( -1.261996585732579224, 4.276409079477648589, -5.312499998634406140 ) ) ;
#9123 = ORIENTED_EDGE ( 'NONE', *, *, #11925, .F. ) ;
#9124 = CARTESIAN_POINT ( 'NONE',  ( 7.922281120364393914, -4.573931137438281169, -8.047472243342932430 ) ) ;
#9125 = VERTEX_POINT ( 'NONE', #1164 ) ;
#9126 = ORIENTED_EDGE ( 'NONE', *, *, #8865, .T. ) ;
#9127 = ADVANCED_FACE ( 'NONE', ( #7321 ), #15424, .T. ) ;
#9128 = ORIENTED_EDGE ( 'NONE', *, *, #4009, .T. ) ;
#9129 = CARTESIAN_POINT ( 'NONE',  ( -4.458734125000000326, -31.25000000136559564, -1.846868145590735644 ) ) ;
#9130 = CARTESIAN_POINT ( 'NONE',  ( 7.102951435054648059E-15, 40.00000000000000000, 57.99999999999999289 ) ) ;
#9131 = ORIENTED_EDGE ( 'NONE', *, *, #15493, .T. ) ;
#9132 = VECTOR ( 'NONE', #11231, 1000.000000000000114 ) ;
#9133 = CARTESIAN_POINT ( 'NONE',  ( -41.99999999999978684, -9.000000000000001776, -3.500000000000001776 ) ) ;
#9134 = CARTESIAN_POINT ( 'NONE',  ( 2.500000000000000000, 0.000000000000000000, 0.000000000000000000 ) ) ;
#9135 = CARTESIAN_POINT ( 'NONE',  ( -3.916244202832140253, 2.131511515620587272, -2.937499998634407472 ) ) ;
#9136 = CARTESIAN_POINT ( 'NONE',  ( 1.865935176646638549, 4.058319590311958436, -0.3789984458506300835 ) ) ;
#9137 = CARTESIAN_POINT ( 'NONE',  ( -5.000000000000000888, -27.56250000000000000, -2.071067811865475949 ) ) ;
#9138 = CARTESIAN_POINT ( 'NONE',  ( -3.753672977998669946, -3.033343224707661712, -1.749999998634408360 ) ) ;
#9139 = DIRECTION ( 'NONE',  ( 0.000000000000000000, 0.000000000000000000, 1.000000000000000000 ) ) ;
#9140 = MANIFOLD_SOLID_BREP ( 'Cavity1', #6899 ) ;
#9141 = CARTESIAN_POINT ( 'NONE',  ( 4.769696007084728073, -20.00000000000000000, 1.500000000000000000 ) ) ;
#9142 = CARTESIAN_POINT ( 'NONE',  ( 5.000000000000000000, -25.18750000273119127, 2.071067811865478614 ) ) ;
#9143 = FACE_OUTER_BOUND ( 'NONE', #3989, .T. ) ;
#9144 = CARTESIAN_POINT ( 'NONE',  ( 4.458734124999999437, -25.37500000136559564, -1.846868145590734978 ) ) ;
#9145 = CARTESIAN_POINT ( 'NONE',  ( -4.999999999999847233, 1.272547481429013860, -6.586597482644652501 ) ) ;
#9146 = VERTEX_POINT ( 'NONE', #6269 ) ;
#9147 = ORIENTED_EDGE ( 'NONE', *, *, #2172, .F. ) ;
#9148 = CARTESIAN_POINT ( 'NONE',  ( 0.6937372685066666156, -4.453844082567737672, -3.610536846335894445 ) ) ;
#9149 = ORIENTED_EDGE ( 'NONE', *, *, #8609, .F. ) ;
#9150 = DIRECTION ( 'NONE',  ( 1.000000000000000000, 0.000000000000000000, 1.114413700119375779E-16 ) ) ;
#9151 =( BOUNDED_CURVE ( )  B_SPLINE_CURVE ( 3, ( #15785, #8518, #2496, #4780 ),
 .UNSPECIFIED., .F., .F. ) 
 B_SPLINE_CURVE_WITH_KNOTS ( ( 4, 4 ),
 ( 3.141592653589793116, 4.712388980384689674 ),
 .UNSPECIFIED. ) 
 CURVE ( )  GEOMETRIC_REPRESENTATION_ITEM ( )  RATIONAL_B_SPLINE_CURVE ( ( 1.000000000000000000, 0.8047378541243649375, 0.8047378541243649375, 1.000000000000000000 ) ) 
 REPRESENTATION_ITEM ( '' )  );
#9152 = ORIENTED_EDGE ( 'NONE', *, *, #11942, .F. ) ;
#9153 = CARTESIAN_POINT ( 'NONE',  ( -28.86751345948129099, -20.00000000000000000, 18.00000000000000000 ) ) ;
#9154 = CYLINDRICAL_SURFACE ( 'NONE', #10402, 5.000000000000000000 ) ;
#9155 = CARTESIAN_POINT ( 'NONE',  ( 4.458734124999999437, -27.75000000136559564, 1.846868145590737864 ) ) ;
#9156 = PRESENTATION_LAYER_ASSIGNMENT (  '', '', ( #5009 ) ) ;
#9157 = CARTESIAN_POINT ( 'NONE',  ( -21.01110699893041911, -3.000000000000000000, -33.74230484541335073 ) ) ;
#9158 = EDGE_CURVE ( 'NONE', #13539, #3896, #11639, .T. ) ;
#9159 = AXIS2_PLACEMENT_3D ( 'NONE', #10661, #3305, #11931 ) ;
#9160 = CYLINDRICAL_SURFACE ( 'NONE', #11556, 9.999999999999998224 ) ;
#9161 = DIRECTION ( 'NONE',  ( 0.000000000000000000, -1.000000000000000000, 0.000000000000000000 ) ) ;
#9162 = VERTEX_POINT ( 'NONE', #1325 ) ;
#9163 = ORIENTED_EDGE ( 'NONE', *, *, #6286, .F. ) ;
#9164 = CARTESIAN_POINT ( 'NONE',  ( 1.846868145590736310, -29.62500000136559208, 4.458734124999999437 ) ) ;
#9165 = AXIS2_PLACEMENT_3D ( 'NONE', #14650, #4875, #3484 ) ;
#9166 = ORIENTED_EDGE ( 'NONE', *, *, #9463, .F. ) ;
#9167 = CIRCLE ( 'NONE', #4773, 2.000000000000000888 ) ;
#9168 = DIRECTION ( 'NONE',  ( 0.000000000000000000, 1.000000000000000000, 0.000000000000000000 ) ) ;
#9169 = EDGE_CURVE ( 'NONE', #7938, #8470, #13600, .T. ) ;
#9170 = CYLINDRICAL_SURFACE ( 'NONE', #12819, 3.499999999999999556 ) ;
#9171 = ADVANCED_FACE ( 'NONE', ( #10145 ), #11183, .T. ) ;
#9172 = PRESENTATION_LAYER_ASSIGNMENT (  '', '', ( #141 ) ) ;
#9173 = STYLED_ITEM ( 'NONE', ( #824 ), #14368 ) ;
#9174 = CARTESIAN_POINT ( 'NONE',  ( -4.209348295687703967, -3.401574460001763001, -7.312499997268814944 ) ) ;
#9175 = DIRECTION ( 'NONE',  ( 0.000000000000000000, 0.000000000000000000, 1.000000000000000000 ) ) ;
#9176 = DIRECTION ( 'NONE',  ( 0.8660254037844383745, -0.000000000000000000, 0.5000000000000004441 ) ) ;
#9177 = CARTESIAN_POINT ( 'NONE',  ( 4.458734124999997661, -23.75000000136559564, 1.846868145590737864 ) ) ;
#9178 = ORIENTED_EDGE ( 'NONE', *, *, #473, .T. ) ;
#9179 = CIRCLE ( 'NONE', #6078, 6.000000000000000888 ) ;
#9180 = LINE ( 'NONE', #1968, #15174 ) ;
#9181 = DIRECTION ( 'NONE',  ( -0.000000000000000000, -0.000000000000000000, 1.000000000000000000 ) ) ;
#9182 = CARTESIAN_POINT ( 'NONE',  ( -9.184850993605147944E-16, -26.37500000273118417, 5.000000000000000000 ) ) ;
#9183 = ORIENTED_EDGE ( 'NONE', *, *, #5753, .F. ) ;
#9184 = CARTESIAN_POINT ( 'NONE',  ( 0.000000000000000000, 0.000000000000000000, -9.999999999999998224 ) ) ;
#9185 = ORIENTED_EDGE ( 'NONE', *, *, #3035, .F. ) ;
#9186 = VERTEX_POINT ( 'NONE', #10230 ) ;
#9187 = CARTESIAN_POINT ( 'NONE',  ( -2.000000000000002665, -3.464101615137770374, -3.142992957459237680 ) ) ;
#9188 = CIRCLE ( 'NONE', #11238, 75.00000000000004263 ) ;
#9189 = CARTESIAN_POINT ( 'NONE',  ( -2.500000000000000888, 0.000000000000000000, -4.974599999999998801 ) ) ;
#9190 = AXIS2_PLACEMENT_3D ( 'NONE', #12921, #10674, #1854 ) ;
#9191 = AXIS2_PLACEMENT_3D ( 'NONE', #10525, #13085, #11872 ) ;
#9192 = APPLICATION_CONTEXT ( 'automotive_design' ) ;
#9193 = ADVANCED_FACE ( 'NONE', ( #6195 ), #4351, .F. ) ;
#9194 = LINE ( 'NONE', #14199, #3786 ) ;
#9195 = DIRECTION ( 'NONE',  ( 0.000000000000000000, 0.000000000000000000, -1.000000000000000000 ) ) ;
#9196 = ADVANCED_FACE ( 'NONE', ( #128 ), #11112, .T. ) ;
#9197 = CARTESIAN_POINT ( 'NONE',  ( 0.000000000000000000, 0.000000000000000000, -4.694516984716113228 ) ) ;
#9198 = CARTESIAN_POINT ( 'NONE',  ( 35.00000000000000000, 40.00000000000000000, 5.999999999999991118 ) ) ;
#9199 = DIRECTION ( 'NONE',  ( 0.8660254037844383745, 0.000000000000000000, 0.5000000000000004441 ) ) ;
#9200 = CARTESIAN_POINT ( 'NONE',  ( -99.99999999999998579, -10.00000000000000888, 7.500000000000001776 ) ) ;
#9201 = CARTESIAN_POINT ( 'NONE',  ( 4.458734124999999437, -21.43750000136559208, 0.000000000000000000 ) ) ;
#9202 = CARTESIAN_POINT ( 'NONE',  ( 4.799145180956616130, -0.5093500532425063732, -5.624999998634406140 ) ) ;
#9203 = VERTEX_POINT ( 'NONE', #2614 ) ;
#9204 = VECTOR ( 'NONE', #866, 1000.000000000000000 ) ;
#9205 = CARTESIAN_POINT ( 'NONE',  ( 44.82050807568879947, 0.000000000000000000, -37.63139720814411504 ) ) ;
#9206 = ORIENTED_EDGE ( 'NONE', *, *, #14897, .T. ) ;
#9207 = EDGE_LOOP ( 'NONE', ( #9537, #3844, #2667, #4476, #8640 ) ) ;
#9208 = CARTESIAN_POINT ( 'NONE',  ( 4.458734124999999437, -29.75000000136559564, 1.846868145590737864 ) ) ;
#9209 = CARTESIAN_POINT ( 'NONE',  ( 10.39117206796836079, 1.272551561242683567E-15, -8.499999999999996447 ) ) ;
#9210 = VERTEX_POINT ( 'NONE', #6436 ) ;
#9211 = CARTESIAN_POINT ( 'NONE',  ( -9.184850993605147944E-16, -28.25000000000000000, 5.000000000000000000 ) ) ;
#9212 = DIRECTION ( 'NONE',  ( -0.000000000000000000, 1.000000000000000000, -0.000000000000000000 ) ) ;
#9213 = CARTESIAN_POINT ( 'NONE',  ( 2.131511515620586383, 3.916244202832140253, -5.187499998634406140 ) ) ;
#9214 = CARTESIAN_POINT ( 'NONE',  ( -67.50000000000000000, 37.00000000000000000, -7.070249711157346244E-13 ) ) ;
#9215 = AXIS2_PLACEMENT_3D ( 'NONE', #10081, #8868, #5465 ) ;
#9216 = EDGE_CURVE ( 'NONE', #2292, #10237, #4081, .T. ) ;
#9217 = CARTESIAN_POINT ( 'NONE',  ( 5.000000000000000000, -25.00000000000000000, 0.000000000000000000 ) ) ;
#9218 = CARTESIAN_POINT ( 'NONE',  ( -4.799145180956616130, 0.5093500532425063732, -7.874999998634408804 ) ) ;
#9219 = PLANE ( 'NONE',  #13501 ) ;
#9220 = CARTESIAN_POINT ( 'NONE',  ( 19.99999999999956657, -8.786575603324269439E-13, -13.00000000000000000 ) ) ;
#9221 = CARTESIAN_POINT ( 'NONE',  ( 5.000000000000000888, -25.06250000273118417, -2.071067811865475505 ) ) ;
#9222 = ORIENTED_EDGE ( 'NONE', *, *, #1950, .T. ) ;
#9223 = CARTESIAN_POINT ( 'NONE',  ( -1.846868145590737420, -25.75000000136559564, 4.458734124999997661 ) ) ;
#9224 = CARTESIAN_POINT ( 'NONE',  ( 5.000000000000095923, 0.7223674278660565662, -7.021799365517158442 ) ) ;
#9225 = EDGE_LOOP ( 'NONE', ( #8685, #4323, #10005, #6012 ) ) ;
#9226 = CIRCLE ( 'NONE', #8453, 2.041999999999999815 ) ;
#9227 = ORIENTED_EDGE ( 'NONE', *, *, #15781, .F. ) ;
#9228 = EDGE_LOOP ( 'NONE', ( #9410, #7343, #2843, #12177 ) ) ;
#9229 = CARTESIAN_POINT ( 'NONE',  ( -43.89750408695873318, -2.999999999999999112, 21.87156796334076247 ) ) ;
#9230 = ORIENTED_EDGE ( 'NONE', *, *, #4162, .F. ) ;
#9231 = VECTOR ( 'NONE', #4207, 1000.000000000000000 ) ;
#9232 = ORIENTED_EDGE ( 'NONE', *, *, #15833, .F. ) ;
#9233 = CARTESIAN_POINT ( 'NONE',  ( 9.999999999999891642, -20.00000000000000000, -19.82050807568883499 ) ) ;
#9234 = AXIS2_PLACEMENT_3D ( 'NONE', #9329, #6672, #4471 ) ;
#9235 = CARTESIAN_POINT ( 'NONE',  ( 0.000000000000000000, -13.00000000000000178, -25.00000000000000000 ) ) ;
#9236 = ADVANCED_FACE ( 'NONE', ( #11350 ), #9893, .T. ) ;
#9237 = CARTESIAN_POINT ( 'NONE',  ( 4.458734124999999437, -28.68750000136559564, 0.000000000000000000 ) ) ;
#9238 = CARTESIAN_POINT ( 'NONE',  ( 2.390265326283148806, 4.391654775818395251, -6.749999997268815832 ) ) ;
#9239 = CARTESIAN_POINT ( 'NONE',  ( 5.000000000000003553, 1.275685995473128912E-14, -5.920263044861758139 ) ) ;
#9240 = APPLICATION_PROTOCOL_DEFINITION ( 'draft international standard', 'automotive_design', 1998, #3609 ) ;
#9241 = AXIS2_PLACEMENT_3D ( 'NONE', #7052, #4860, #4618 ) ;
#9242 = CARTESIAN_POINT ( 'NONE',  ( 7.500000000000003553, -4.330127018922199866, -7.422398894150035176 ) ) ;
#9243 = DIRECTION ( 'NONE',  ( 1.000000000000000000, 0.000000000000000000, 0.000000000000000000 ) ) ;
#9244 = ORIENTED_EDGE ( 'NONE', *, *, #8278, .F. ) ;
#9245 =( BOUNDED_CURVE ( )  B_SPLINE_CURVE ( 2, ( #10710, #13034, #1977, #6923, #11828, #777, #10636, #15646, #4564, #9498, #14430, #3355, #14740, #15963, #1008, #9726, #7477, #8375, #5939, #10863, #12061, #12381, #1316, #6260, #15804, #4884, #13353, #14662, #5038, #117, #13266, #11175, #9968, #13589, #11104, #2438, #3422, #14574, #1153, #9811, #3497, #6095, #11024, #13425, #12298, #2208, #7160, #2518, #4720, #3589, #8535, #9640, #7313, #8456, #2363, #12215, #2294, #3662, #4800, #1234, #8605, #6185, #7242, #12139, #42, #13500, #4956, #7390, #9884, #14816, #3741, #1078, #6015, #8686, #10940, #15879, #12694, #12458, #11414, #4142, #2684, #13839, #9015, #15063, #14988, #1564, #7642, #13752, #13674, #11258, #2605, #2770, #10059, #14909, #12537, #1637, #13921, #5279, #10307, #5127, #8930, #289, #1482, #7727, #12623, #5202, #10219, #7558, #1394, #6576, #5367, #10133, #3977, #11493, #6502, #3901, #363, #15143, #440, #4063, #6426, #2848, #7802, #15231, #8847, #208, #3827, #8771, #6340, #11342, #13558, #5008, #2410 ),
 .UNSPECIFIED., .F., .F. ) 
 B_SPLINE_CURVE_WITH_KNOTS ( ( 3, 2, 2, 2, 2, 2, 2, 2, 2, 2, 2, 2, 2, 2, 2, 2, 2, 2, 2, 2, 2, 2, 2, 2, 2, 2, 2, 2, 2, 2, 2, 2, 2, 2, 2, 2, 2, 2, 2, 2, 2, 2, 2, 2, 2, 2, 2, 2, 2, 2, 2, 2, 2, 2, 2, 2, 2, 2, 2, 2, 2, 2, 2, 2, 2, 2, 3 ),
 ( 0.1816346841896726849, 0.1875000000000000000, 0.2000000000000000111, 0.2124999999999999944, 0.2250000000000000056, 0.2374999999999999889, 0.2500000000000000000, 0.2625000000000000111, 0.2750000000000000222, 0.2874999999999999778, 0.2999999999999999889, 0.3125000000000000000, 0.3250000000000000111, 0.3375000000000000222, 0.3499999999999999778, 0.3624999999999999889, 0.3750000000000000000, 0.3875000000000000111, 0.4000000000000000222, 0.4124999999999999778, 0.4250000000000000444, 0.4375000000000000000, 0.4499999999999999556, 0.4625000000000000222, 0.4749999999999999778, 0.4875000000000000444, 0.5000000000000000000, 0.5124999999999999556, 0.5250000000000000222, 0.5374999999999999778, 0.5500000000000000444, 0.5625000000000000000, 0.5749999999999999556, 0.5875000000000000222, 0.5999999999999999778, 0.6125000000000000444, 0.6250000000000000000, 0.6374999999999999556, 0.6500000000000000222, 0.6624999999999999778, 0.6750000000000001554, 0.6875000000000000000, 0.6999999999999999556, 0.7125000000000000222, 0.7249999999999999778, 0.7375000000000000444, 0.7500000000000000000, 0.7624999999999999556, 0.7750000000000000222, 0.7874999999999999778, 0.8000000000000000444, 0.8125000000000000000, 0.8249999999999999556, 0.8375000000000000222, 0.8499999999999999778, 0.8625000000000000444, 0.8750000000000000000, 0.8874999999999999556, 0.8999999999999999112, 0.9124999999999999778, 0.9250000000000000444, 0.9375000000000000000, 0.9499999999999999556, 0.9624999999999999112, 0.9749999999999999778, 0.9875000000000000444, 1.000000000000000000 ),
 .UNSPECIFIED. ) 
 CURVE ( )  GEOMETRIC_REPRESENTATION_ITEM ( )  RATIONAL_B_SPLINE_CURVE ( ( 0.9620839512587866516, 0.9642823534839155553, 1.000000000000000000, 0.9238795325112867385, 1.000000000000000000, 0.9238795325112867385, 1.000000000000000000, 0.9238795325112867385, 1.000000000000000000, 0.9238795325112867385, 1.000000000000000000, 0.9238795325112867385, 1.000000000000000000, 0.9238795325112867385, 1.000000000000000000, 0.9238795325112867385, 1.000000000000000000, 0.9238795325112867385, 1.000000000000000000, 0.9238795325112867385, 1.000000000000000000, 0.9238795325112867385, 1.000000000000000000, 0.9238795325112867385, 1.000000000000000000, 0.9238795325112867385, 1.000000000000000000, 0.9238795325112867385, 1.000000000000000000, 0.9238795325112867385, 1.000000000000000000, 0.9238795325112867385, 1.000000000000000000, 0.9238795325112867385, 1.000000000000000000, 0.9238795325112867385, 1.000000000000000000, 0.9238795325112867385, 1.000000000000000000, 0.9238795325112867385, 1.000000000000000000, 0.9238795325112867385, 1.000000000000000000, 0.9238795325112867385, 1.000000000000000000, 0.9238795325112867385, 1.000000000000000000, 0.9238795325112867385, 1.000000000000000000, 0.9238795325112867385, 1.000000000000000000, 0.9238795325112867385, 1.000000000000000000, 0.9238795325112867385, 1.000000000000000000, 0.9238795325112867385, 1.000000000000000000, 0.9238795325112867385, 1.000000000000000000, 0.9238795325112867385, 1.000000000000000000, 0.9238795325112867385, 1.000000000000000000, 0.9238795325112867385, 1.000000000000000000, 0.9238795325112867385, 1.000000000000000000, 0.9238795325112867385, 1.000000000000000000, 0.9238795325112867385, 1.000000000000000000, 0.9238795325112867385, 1.000000000000000000, 0.9238795325112867385, 1.000000000000000000, 0.9238795325112867385, 1.000000000000000000, 0.9238795325112867385, 1.000000000000000000, 0.9238795325112867385, 1.000000000000000000, 0.9238795325112867385, 1.000000000000000000, 0.9238795325112867385, 1.000000000000000000, 0.9238795325112867385, 1.000000000000000000, 0.9238795325112867385, 1.000000000000000000, 0.9238795325112867385, 1.000000000000000000, 0.9238795325112867385, 1.000000000000000000, 0.9238795325112867385, 1.000000000000000000, 0.9238795325112867385, 1.000000000000000000, 0.9238795325112867385, 1.000000000000000000, 0.9238795325112867385, 1.000000000000000000, 0.9238795325112867385, 1.000000000000000000, 0.9238795325112867385, 1.000000000000000000, 0.9238795325112867385, 1.000000000000000000, 0.9238795325112867385, 1.000000000000000000, 0.9238795325112867385, 1.000000000000000000, 0.9238795325112867385, 1.000000000000000000, 0.9238795325112867385, 1.000000000000000000, 0.9238795325112867385, 1.000000000000000000, 0.9238795325112867385, 1.000000000000000000, 0.9238795325112867385, 1.000000000000000000, 0.9238795325112867385, 1.000000000000000000, 0.9238795325112867385, 1.000000000000000000, 0.9238795325112867385, 1.000000000000000000, 0.9238795325112867385, 1.000000000000000000, 0.9238795325112867385, 1.000000000000000000, 0.9238795325112867385, 1.000000000000000000 ) ) 
 REPRESENTATION_ITEM ( '' )  );
#9246 = CIRCLE ( 'NONE', #11295, 2.649999999999992806 ) ;
#9247 = ORIENTED_EDGE ( 'NONE', *, *, #13260, .F. ) ;
#9248 = CARTESIAN_POINT ( 'NONE',  ( -7.779103221381285849, 4.168986698926044454, -7.929128246061914354 ) ) ;
#9249 = PRESENTATION_LAYER_ASSIGNMENT (  '', '', ( #3506 ) ) ;
#9250 = ORIENTED_EDGE ( 'NONE', *, *, #4567, .F. ) ;
#9251 = ADVANCED_FACE ( 'NONE', ( #5049 ), #1497, .T. ) ;
#9252 = CONICAL_SURFACE ( 'NONE', #12070, 2.041999999999999815, 1.047197551196591858 ) ;
#9253 = DIRECTION ( 'NONE',  ( 0.000000000000000000, 0.000000000000000000, 1.000000000000000000 ) ) ;
#9254 = ORIENTED_EDGE ( 'NONE', *, *, #4643, .F. ) ;
#9255 = DIRECTION ( 'NONE',  ( -0.000000000000000000, -0.000000000000000000, -1.000000000000000000 ) ) ;
#9256 = STYLED_ITEM ( 'NONE', ( #6108 ), #9113 ) ;
#9257 = CARTESIAN_POINT ( 'NONE',  ( 0.000000000000000000, 0.000000000000000000, 3.469446951953614189E-15 ) ) ;
#9258 = CARTESIAN_POINT ( 'NONE',  ( -1.261996585732579224, 4.276409079477648589, 0.6875000013655923059 ) ) ;
#9259 = DIRECTION ( 'NONE',  ( 0.000000000000000000, 0.000000000000000000, -1.000000000000000000 ) ) ;
#9260 = CARTESIAN_POINT ( 'NONE',  ( -1.415196051561583790, 4.795541693661363958, -1.750000000000001554 ) ) ;
#9261 = CARTESIAN_POINT ( 'NONE',  ( -44.99999999999999289, -11.00000000000000178, 4.000000000000831335 ) ) ;
#9262 = VERTEX_POINT ( 'NONE', #2532 ) ;
#9263 = PLANE ( 'NONE',  #6400 ) ;
#9264 = LINE ( 'NONE', #7972, #12538 ) ;
#9265 = ORIENTED_EDGE ( 'NONE', *, *, #10379, .F. ) ;
#9266 = CARTESIAN_POINT ( 'NONE',  ( 12.67949192431120586, -37.00000000000000711, 61.96152422706632024 ) ) ;
#9267 = ORIENTED_EDGE ( 'NONE', *, *, #14135, .F. ) ;
#9268 = ORIENTED_EDGE ( 'NONE', *, *, #6237, .T. ) ;
#9269 = EDGE_CURVE ( 'NONE', #11087, #7869, #3987, .T. ) ;
#9270 = CARTESIAN_POINT ( 'NONE',  ( 42.02221399786069611, 2.000000000000000000, 1.075528555105620399E-13 ) ) ;
#9271 = AXIS2_PLACEMENT_3D ( 'NONE', #9197, #9278, #705 ) ;
#9272 = ADVANCED_FACE ( 'NONE', ( #9097 ), #6677, .F. ) ;
#9273 = CIRCLE ( 'NONE', #13371, 2.649999999999985700 ) ;
#9274 = CARTESIAN_POINT ( 'NONE',  ( 10.17949192431126448, -5.000000000000000000, -57.63139720814413636 ) ) ;
#9275 = VECTOR ( 'NONE', #7481, 1000.000000000000000 ) ;
#9276 = CYLINDRICAL_SURFACE ( 'NONE', #6123, 32.00000000000000711 ) ;
#9277 = CARTESIAN_POINT ( 'NONE',  ( 3.061616997868383141E-16, -25.75000000000000355, -5.000000000000000000 ) ) ;
#9278 = DIRECTION ( 'NONE',  ( -0.000000000000000000, -0.000000000000000000, 1.000000000000000000 ) ) ;
#9279 = CARTESIAN_POINT ( 'NONE',  ( -16.18981371719892692, -5.000000000000000000, 15.95842007673591745 ) ) ;
#9280 = CARTESIAN_POINT ( 'NONE',  ( 35.00000000000000000, 40.00000000000000000, -5.999999999999991118 ) ) ;
#9281 = VECTOR ( 'NONE', #5595, 1000.000000000000114 ) ;
#9282 = DIRECTION ( 'NONE',  ( 0.000000000000000000, 0.000000000000000000, 1.000000000000000000 ) ) ;
#9283 = CARTESIAN_POINT ( 'NONE',  ( 4.458734124999999437, -31.62500000136559564, -1.846868145590734978 ) ) ;
#9284 = CIRCLE ( 'NONE', #11330, 2.500000000000909495 ) ;
#9285 = CARTESIAN_POINT ( 'NONE',  ( 1.261996585732578113, -4.276409079477644148, 1.437500001365592972 ) ) ;
#9286 = ORIENTED_EDGE ( 'NONE', *, *, #11418, .T. ) ;
#9287 = CARTESIAN_POINT ( 'NONE',  ( 4.859103478305521033E-15, 8.660254037844390851, -7.564335161054499324 ) ) ;
#9288 = ORIENTED_EDGE ( 'NONE', *, *, #14488, .T. ) ;
#9289 = EDGE_LOOP ( 'NONE', ( #8392, #9456, #3696, #8567 ) ) ;
#9290 = CARTESIAN_POINT ( 'NONE',  ( -3.152801135295367096, -25.31250000136559564, -3.152801135295367541 ) ) ;
#9291 = DIRECTION ( 'NONE',  ( -1.000000000000000000, 1.224646799147352714E-16, 0.000000000000000000 ) ) ;
#9292 = EDGE_CURVE ( 'NONE', #10281, #1816, #11817, .T. ) ;
#9293 = ORIENTED_EDGE ( 'NONE', *, *, #11352, .F. ) ;
#9294 = CARTESIAN_POINT ( 'NONE',  ( -5.000000000000002665, -1.404940523648820476E-14, -6.545263047592945860 ) ) ;
#9295 = AXIS2_PLACEMENT_3D ( 'NONE', #3659, #112, #5034 ) ;
#9296 = CARTESIAN_POINT ( 'NONE',  ( -55.00000000000000000, -10.00000000000000178, 17.50000000000000000 ) ) ;
#9297 = CARTESIAN_POINT ( 'NONE',  ( 3.753672977998667726, 3.033343224707664820, -6.249999998634408804 ) ) ;
#9298 = DIRECTION ( 'NONE',  ( -0.000000000000000000, 1.000000000000000000, -0.000000000000000000 ) ) ;
#9299 = CARTESIAN_POINT ( 'NONE',  ( 3.535533905932738197, -25.87500000000000355, -3.535533905932738197 ) ) ;
#9300 = CARTESIAN_POINT ( 'NONE',  ( -3.916244202832140253, 2.131511515620587272, -7.937499998634408804 ) ) ;
#9301 = DIRECTION ( 'NONE',  ( -0.000000000000000000, -0.000000000000000000, -1.000000000000000000 ) ) ;
#9302 = DIRECTION ( 'NONE',  ( -1.734723475976807489E-15, 0.000000000000000000, 1.000000000000000000 ) ) ;
#9303 = CARTESIAN_POINT ( 'NONE',  ( -5.000000000000000888, -23.56250000273118417, 2.071067811865474617 ) ) ;
#9304 = EDGE_LOOP ( 'NONE', ( #13905, #420 ) ) ;
#9305 = CARTESIAN_POINT ( 'NONE',  ( 1.846868145590735200, -26.25000000136559564, -4.458734124999999437 ) ) ;
#9306 = CARTESIAN_POINT ( 'NONE',  ( 0.2500000000000002220, 0.000000000000000000, 4.000000000000000000 ) ) ;
#9307 = ORIENTED_EDGE ( 'NONE', *, *, #2866, .T. ) ;
#9308 = EDGE_LOOP ( 'NONE', ( #14595, #12897, #3588, #9565 ) ) ;
#9309 = CARTESIAN_POINT ( 'NONE',  ( 5.000000000000004441, -2.247904837838113790E-16, -3.920263044861760360 ) ) ;
#9310 = EDGE_CURVE ( 'NONE', #11317, #9517, #5689, .T. ) ;
#9311 = CYLINDRICAL_SURFACE ( 'NONE', #15124, 4.250000000000000000 ) ;
#9312 = ADVANCED_FACE ( 'NONE', ( #8128 ), #1884, .T. ) ;
#9313 = EDGE_CURVE ( 'NONE', #5664, #5600, #13571, .T. ) ;
#9314 = ORIENTED_EDGE ( 'NONE', *, *, #11198, .F. ) ;
#9315 = DIRECTION ( 'NONE',  ( 1.000000000000000000, 1.239088197126290324E-16, 0.000000000000000000 ) ) ;
#9316 = CARTESIAN_POINT ( 'NONE',  ( 39.53738644055469820, -5.000000000000000000, -28.48076211352550047 ) ) ;
#9317 = CARTESIAN_POINT ( 'NONE',  ( 4.458734124999999437, -27.68750000136559564, 0.000000000000000000 ) ) ;
#9318 = CARTESIAN_POINT ( 'NONE',  ( 2.742827927723449299, 3.035229711104609596, -3.433252694550591233 ) ) ;
#9319 = CARTESIAN_POINT ( 'NONE',  ( 17.99999999999957012, -8.784126309725975241E-13, -4.500000000000000000 ) ) ;
#9320 = CARTESIAN_POINT ( 'NONE',  ( 0.5093500532425063732, 4.799145180956616130, -8.374999998634409692 ) ) ;
#9321 = CARTESIAN_POINT ( 'NONE',  ( 0.5093500532425063732, 4.799145180956616130, -0.3749999986344090264 ) ) ;
#9322 = ORIENTED_EDGE ( 'NONE', *, *, #7113, .F. ) ;
#9323 = ORIENTED_EDGE ( 'NONE', *, *, #8182, .F. ) ;
#9324 = CARTESIAN_POINT ( 'NONE',  ( 0.000000000000000000, -20.00000000000000000, 0.000000000000000000 ) ) ;
#9325 = EDGE_CURVE ( 'NONE', #14420, #4500, #15397, .T. ) ;
#9326 = ORIENTED_EDGE ( 'NONE', *, *, #4746, .F. ) ;
#9327 = CARTESIAN_POINT ( 'NONE',  ( 5.000000000000000000, -21.56250000136559208, 0.000000000000000000 ) ) ;
#9328 = CARTESIAN_POINT ( 'NONE',  ( 39.61557500986572933, -4.342938577511704423, 28.40349439876419169 ) ) ;
#9329 = CARTESIAN_POINT ( 'NONE',  ( 0.000000000000000000, 0.000000000000000000, -9.999999999999998224 ) ) ;
#9330 =( BOUNDED_CURVE ( )  B_SPLINE_CURVE ( 2, ( #6362, #11282, #6688, #10394, #12643, #1581, #11596, #380, #1507, #11434, #5300 ),
 .UNSPECIFIED., .F., .F. ) 
 B_SPLINE_CURVE_WITH_KNOTS ( ( 3, 2, 2, 2, 2, 3 ),
 ( 0.2045872658012772849, 0.2124999999999999944, 0.2250000000000000056, 0.2374999999999999889, 0.2500000000000000000, 0.2545872658012772738 ),
 .UNSPECIFIED. ) 
 CURVE ( )  GEOMETRIC_REPRESENTATION_ITEM ( )  RATIONAL_B_SPLINE_CURVE ( ( 0.9646335149384808183, 0.9518143178943438976, 1.000000000000000000, 0.9238795325112867385, 1.000000000000000000, 0.9238795325112867385, 1.000000000000000000, 0.9238795325112867385, 1.000000000000000000, 0.9720652146169430630, 0.9646335149384808183 ) ) 
 REPRESENTATION_ITEM ( '' )  );
#9331 = CARTESIAN_POINT ( 'NONE',  ( -3.401574460001764777, 4.209348295687701302, -6.562499997268814944 ) ) ;
#9332 = LINE ( 'NONE', #14096, #10074 ) ;
#9333 = SURFACE_STYLE_USAGE ( .BOTH. , #6585 ) ;
#9334 = DIRECTION ( 'NONE',  ( -1.000000000000000000, -0.000000000000000000, -0.000000000000000000 ) ) ;
#9335 = VERTEX_POINT ( 'NONE', #12705 ) ;
#9336 = DIRECTION ( 'NONE',  ( 0.000000000000000000, -1.000000000000000000, 0.000000000000000000 ) ) ;
#9337 = CARTESIAN_POINT ( 'NONE',  ( -7.703920929261746764, 4.447860822324885888, -7.917989418073283048 ) ) ;
#9338 = DIRECTION ( 'NONE',  ( 0.000000000000000000, 0.000000000000000000, 1.000000000000000000 ) ) ;
#9339 = ORIENTED_EDGE ( 'NONE', *, *, #6047, .F. ) ;
#9340 = FACE_OUTER_BOUND ( 'NONE', #6998, .T. ) ;
#9341 = ORIENTED_EDGE ( 'NONE', *, *, #2677, .T. ) ;
#9342 = EDGE_LOOP ( 'NONE', ( #948, #6298, #3023, #10787 ) ) ;
#9343 = CARTESIAN_POINT ( 'NONE',  ( 0.000000000000000000, -20.00000000000000000, 0.000000000000000000 ) ) ;
#9344 = DIRECTION ( 'NONE',  ( 0.000000000000000000, 0.000000000000000000, 1.000000000000000000 ) ) ;
#9345 = DIRECTION ( 'NONE',  ( 0.000000000000000000, 1.000000000000000000, 0.000000000000000000 ) ) ;
#9346 = MANIFOLD_SOLID_BREP ( 'M5 Clearance Hole1', #13312 ) ;
#9347 = CARTESIAN_POINT ( 'NONE',  ( 2.071067811865461294, -25.93750000273118062, -5.000000000000014211 ) ) ;
#9348 = FACE_OUTER_BOUND ( 'NONE', #13787, .T. ) ;
#9349 = CARTESIAN_POINT ( 'NONE',  ( 4.458734124999998549, -3.052311964297492742E-11, -0.3789984458506765463 ) ) ;
#9350 = DIRECTION ( 'NONE',  ( -0.4999999999999997780, -0.000000000000000000, -0.8660254037844389297 ) ) ;
#9351 = DIRECTION ( 'NONE',  ( -0.000000000000000000, -1.000000000000000000, -0.000000000000000000 ) ) ;
#9352 = ADVANCED_FACE ( 'NONE', ( #12782 ), #11732, .F. ) ;
#9353 = CARTESIAN_POINT ( 'NONE',  ( 3.061616997868383141E-16, -23.87500000273118772, -5.000000000000000000 ) ) ;
#9354 = ADVANCED_FACE ( 'NONE', ( #9408 ), #1726, .F. ) ;
#9355 = CARTESIAN_POINT ( 'NONE',  ( 3.152801135295366208, -28.81250000136559564, 3.152801135295367985 ) ) ;
#9356 = CARTESIAN_POINT ( 'NONE',  ( 4.276409079477644148, 1.261996585732577891, -1.312499998634406140 ) ) ;
#9357 = ORIENTED_EDGE ( 'NONE', *, *, #8511, .F. ) ;
#9358 = UNCERTAINTY_MEASURE_WITH_UNIT (LENGTH_MEASURE( 1.000000000000000082E-05 ), #13509, 'distance_accuracy_value', 'NONE');
#9359 = DIRECTION ( 'NONE',  ( 0.000000000000000000, 0.000000000000000000, -1.000000000000000000 ) ) ;
#9360 = EDGE_LOOP ( 'NONE', ( #2162, #972, #12210 ) ) ;
#9361 = VERTEX_POINT ( 'NONE', #15317 ) ;
#9362 = CARTESIAN_POINT ( 'NONE',  ( 4.458734124999999437, -28.68750000136559564, 0.000000000000000000 ) ) ;
#9363 = CARTESIAN_POINT ( 'NONE',  ( 3.680118525130245732, -2.494084732383344605, -0.3507732604232533524 ) ) ;
#9364 = DIRECTION ( 'NONE',  ( 0.000000000000000000, 0.000000000000000000, 1.000000000000000000 ) ) ;
#9365 = VECTOR ( 'NONE', #9611, 1000.000000000000000 ) ;
#9366 = CARTESIAN_POINT ( 'NONE',  ( 7.500000000000000000, 0.7723602884921818568, -7.026388801733943978 ) ) ;
#9367 = AXIS2_PLACEMENT_3D ( 'NONE', #6928, #7988, #4248 ) ;
#9368 = CARTESIAN_POINT ( 'NONE',  ( -0.5093500532425060401, -4.799145180956616130, -5.624999998634405252 ) ) ;
#9369 = CARTESIAN_POINT ( 'NONE',  ( -5.000000000000004441, -1.011557177027151181E-15, -5.420263044861760804 ) ) ;
#9370 = CARTESIAN_POINT ( 'NONE',  ( -9.184850993605147944E-16, -24.25000000000000000, 5.000000000000000000 ) ) ;
#9371 = CARTESIAN_POINT ( 'NONE',  ( -5.381735091635034607, 0.5711823568785950878, 1.437499999999998446 ) ) ;
#9372 = CARTESIAN_POINT ( 'NONE',  ( 6.123233995736766282E-16, 20.00000000000000000, -5.000000000000000000 ) ) ;
#9373 = EDGE_CURVE ( 'NONE', #7550, #12914, #15129, .T. ) ;
#9374 = DIRECTION ( 'NONE',  ( -0.000000000000000000, -0.000000000000000000, 1.000000000000000000 ) ) ;
#9375 = EDGE_CURVE ( 'NONE', #9048, #6744, #10699, .T. ) ;
#9376 = CARTESIAN_POINT ( 'NONE',  ( 4.458734125000000326, -30.37500000136559564, -1.846868145590734978 ) ) ;
#9377 = ORIENTED_EDGE ( 'NONE', *, *, #3298, .F. ) ;
#9378 = LINE ( 'NONE', #14675, #14402 ) ;
#9379 = CARTESIAN_POINT ( 'NONE',  ( -4.618802153516976539, -4.999999999999997335, -36.00000000000000711 ) ) ;
#9380 = EDGE_LOOP ( 'NONE', ( #5698, #9915, #5741, #4971 ) ) ;
#9381 = VERTEX_POINT ( 'NONE', #4554 ) ;
#9382 = LINE ( 'NONE', #6729, #512 ) ;
#9383 = AXIS2_PLACEMENT_3D ( 'NONE', #8060, #1893, #2058 ) ;
#9384 = FACE_OUTER_BOUND ( 'NONE', #11236, .T. ) ;
#9385 = ORIENTED_EDGE ( 'NONE', *, *, #1140, .T. ) ;
#9386 = DIRECTION ( 'NONE',  ( -0.000000000000000000, -1.000000000000000000, -0.000000000000000000 ) ) ;
#9387 = LINE ( 'NONE', #14310, #12444 ) ;
#9388 = CARTESIAN_POINT ( 'NONE',  ( 4.458734125000000326, -27.62500000136559564, -1.846868145590734978 ) ) ;
#9389 = LINE ( 'NONE', #8189, #4172 ) ;
#9390 = EDGE_CURVE ( 'NONE', #2868, #7896, #3263, .T. ) ;
#9391 = CARTESIAN_POINT ( 'NONE',  ( -21.01110699893060030, 0.000000000000000000, 39.04230484541323420 ) ) ;
#9392 = EDGE_CURVE ( 'NONE', #11894, #13329, #745, .T. ) ;
#9393 = FILL_AREA_STYLE_COLOUR ( '', #2707 ) ;
#9394 = CARTESIAN_POINT ( 'NONE',  ( 3.033343224707661712, -3.753672977998669946, -7.749999998634409692 ) ) ;
#9395 = DIRECTION ( 'NONE',  ( -1.000000000000000000, -0.000000000000000000, -0.000000000000000000 ) ) ;
#9396 = ORIENTED_EDGE ( 'NONE', *, *, #6366, .F. ) ;
#9397 = APPLICATION_PROTOCOL_DEFINITION ( 'draft international standard', 'automotive_design', 1998, #99 ) ;
#9398 = EDGE_LOOP ( 'NONE', ( #12391, #11000, #5219, #7976 ) ) ;
#9399 = LINE ( 'NONE', #15547, #11086 ) ;
#9400 = VERTEX_POINT ( 'NONE', #10781 ) ;
#9401 =( REPRESENTATION_RELATIONSHIP ('NONE','NONE', #4176, #790 ) REPRESENTATION_RELATIONSHIP_WITH_TRANSFORMATION ( #6575 )SHAPE_REPRESENTATION_RELATIONSHIP( ) );
#9402 = SURFACE_SIDE_STYLE ('',( #5605 ) ) ;
#9403 = CARTESIAN_POINT ( 'NONE',  ( 1.654252653721905331, 3.663718938583014229, -0.01223254789873410957 ) ) ;
#9404 = CARTESIAN_POINT ( 'NONE',  ( 14.41154273188013590, -5.000000000000004441, -60.96152422706631313 ) ) ;
#9405 = EDGE_CURVE ( 'NONE', #14954, #11629, #5740, .T. ) ;
#9406 = CARTESIAN_POINT ( 'NONE',  ( -3.401574460001764777, 4.209348295687701302, -7.562499997268814944 ) ) ;
#9407 = LINE ( 'NONE', #14183, #11399 ) ;
#9408 = FACE_OUTER_BOUND ( 'NONE', #2561, .T. ) ;
#9409 = CARTESIAN_POINT ( 'NONE',  ( -21.01110699893060030, -3.000000000000000000, 33.74230484541324415 ) ) ;
#9410 = ORIENTED_EDGE ( 'NONE', *, *, #14245, .F. ) ;
#9411 = FACE_OUTER_BOUND ( 'NONE', #10687, .T. ) ;
#9412 = CARTESIAN_POINT ( 'NONE',  ( 4.209348295687701302, 3.401574460001766109, -2.812499997268815388 ) ) ;
#9413 = MECHANICAL_DESIGN_GEOMETRIC_PRESENTATION_REPRESENTATION (  '', ( #15362 ), #5794 ) ;
#9414 = CARTESIAN_POINT ( 'NONE',  ( -6.762176242291807225E-13, 40.00000000000000000, 70.14999999999930935 ) ) ;
#9415 = ORIENTED_EDGE ( 'NONE', *, *, #6179, .F. ) ;
#9416 = LINE ( 'NONE', #929, #1760 ) ;
#9417 = ORIENTED_EDGE ( 'NONE', *, *, #7517, .F. ) ;
#9418 = AXIS2_PLACEMENT_3D ( 'NONE', #11670, #9345, #7984 ) ;
#9419 = ORIENTED_EDGE ( 'NONE', *, *, #11853, .T. ) ;
#9420 = CARTESIAN_POINT ( 'NONE',  ( 5.000000000000000000, -23.18750000273119127, 2.071067811865478614 ) ) ;
#9421 = DIRECTION ( 'NONE',  ( -0.000000000000000000, 1.000000000000000000, -0.000000000000000000 ) ) ;
#9422 = CARTESIAN_POINT ( 'NONE',  ( -4.406842699996125212, 6.115962218725290001, -6.301925127571993537E-16 ) ) ;
#9423 = LINE ( 'NONE', #10399, #11021 ) ;
#9424 = CARTESIAN_POINT ( 'NONE',  ( -115.0000000000000142, -10.00000000000000888, 17.50000000000000000 ) ) ;
#9425 = VECTOR ( 'NONE', #680, 1000.000000000000000 ) ;
#9426 = EDGE_CURVE ( 'NONE', #15428, #7875, #3350, .T. ) ;
#9427 = CARTESIAN_POINT ( 'NONE',  ( 47.32050807568879947, -37.00000000000000711, -41.96152422706630603 ) ) ;
#9428 = DIRECTION ( 'NONE',  ( -0.8660254037844385966, 0.000000000000000000, 0.5000000000000000000 ) ) ;
#9429 = DIRECTION ( 'NONE',  ( -0.000000000000000000, 0.000000000000000000, -1.000000000000000000 ) ) ;
#9430 = LINE ( 'NONE', #3287, #480 ) ;
#9431 = CARTESIAN_POINT ( 'NONE',  ( -1.846868145590734756, -30.37500000136559564, -4.458734124999999437 ) ) ;
#9432 = CARTESIAN_POINT ( 'NONE',  ( -3.753672977998669946, -3.033343224707661712, 1.250000001365594304 ) ) ;
#9433 = ORIENTED_EDGE ( 'NONE', *, *, #14696, .F. ) ;
#9434 = CARTESIAN_POINT ( 'NONE',  ( 5.174575781540989183, 5.672711317429576461, -7.030005583190789942 ) ) ;
#9435 = VERTEX_POINT ( 'NONE', #6993 ) ;
#9436 = ORIENTED_EDGE ( 'NONE', *, *, #3313, .F. ) ;
#9438 = AXIS2_PLACEMENT_3D ( 'NONE', #11153, #7532, #12434 ) ;
#9437 = FILL_AREA_STYLE ('',( #10653 ) ) ;
#9439 = CARTESIAN_POINT ( 'NONE',  ( -4.458734124999999437, -27.18750000136559564, -5.460374474430324690E-16 ) ) ;
#9440 = LINE ( 'NONE', #1834, #4295 ) ;
#9441 = FACE_OUTER_BOUND ( 'NONE', #135, .T. ) ;
#9442 = EDGE_CURVE ( 'NONE', #1601, #2454, #10111, .T. ) ;
#9443 = CARTESIAN_POINT ( 'NONE',  ( -3.535533905932738641, -29.37500000000000355, 3.535533905932737309 ) ) ;
#9444 = CARTESIAN_POINT ( 'NONE',  ( 0.5093500532425063732, 4.799145180956616130, -7.124999998634407916 ) ) ;
#9445 = CARTESIAN_POINT ( 'NONE',  ( 4.209348295687701302, 3.401574460001766109, -5.812499997268813168 ) ) ;
#9446 = CARTESIAN_POINT ( 'NONE',  ( 5.000000000000000000, -27.00000000000000000, 0.000000000000000000 ) ) ;
#9447 = CARTESIAN_POINT ( 'NONE',  ( 3.916244202832140253, -2.131511515620588160, -6.437499998634407028 ) ) ;
#9448 = DIRECTION ( 'NONE',  ( 0.000000000000000000, 1.000000000000000000, 0.000000000000000000 ) ) ;
#9449 = CARTESIAN_POINT ( 'NONE',  ( 2.000000000000008882, 3.464101615137749945, 0.000000000000000000 ) ) ;
#9450 = CARTESIAN_POINT ( 'NONE',  ( -4.458734125000001214, -29.87500000136559564, 1.846868145590734089 ) ) ;
#9451 = AXIS2_PLACEMENT_3D ( 'NONE', #13210, #4741, #12321 ) ;
#9452 = ORIENTED_EDGE ( 'NONE', *, *, #1485, .F. ) ;
#9453 = CARTESIAN_POINT ( 'NONE',  ( -4.458734124999999437, -23.00000000136559564, -1.846868145590735644 ) ) ;
#9454 = DIRECTION ( 'NONE',  ( -0.000000000000000000, 1.000000000000000000, -0.000000000000000000 ) ) ;
#9455 = ORIENTED_EDGE ( 'NONE', *, *, #102, .F. ) ;
#9456 = ORIENTED_EDGE ( 'NONE', *, *, #11796, .T. ) ;
#9457 = CARTESIAN_POINT ( 'NONE',  ( 7.500000000000000888, -3.640541674360524116, -0.7158139487964624292 ) ) ;
#9458 = CARTESIAN_POINT ( 'NONE',  ( -4.458734124999999437, -26.93750000136559564, -5.460374474430324690E-16 ) ) ;
#9459 = CARTESIAN_POINT ( 'NONE',  ( -115.0000000000000142, -10.00000000000000888, 17.50000000000000000 ) ) ;
#9460 = ORIENTED_EDGE ( 'NONE', *, *, #5449, .F. ) ;
#9461 = CARTESIAN_POINT ( 'NONE',  ( 0.000000000000000000, 0.000000000000000000, 0.000000000000000000 ) ) ;
#9462 = EDGE_CURVE ( 'NONE', #12753, #1232, #5388, .T. ) ;
#9463 = EDGE_CURVE ( 'NONE', #5239, #10374, #12857, .T. ) ;
#9464 = AXIS2_PLACEMENT_3D ( 'NONE', #14759, #1097, #7332 ) ;
#9465 = CARTESIAN_POINT ( 'NONE',  ( 0.000000000000000000, 40.00000000000000000, -75.00000000000004263 ) ) ;
#9466 = CARTESIAN_POINT ( 'NONE',  ( -1.846868145590737420, -28.00000000136559564, 4.458734124999999437 ) ) ;
#9467 = DIRECTION ( 'NONE',  ( 0.000000000000000000, 0.000000000000000000, 1.000000000000000000 ) ) ;
#9468 = AXIS2_PLACEMENT_3D ( 'NONE', #4827, #8633, #6209 ) ;
#9469 = DIRECTION ( 'NONE',  ( 6.938893903907228378E-16, 1.000000000000000000, -0.000000000000000000 ) ) ;
#9470 = DIRECTION ( 'NONE',  ( -1.000000000000000000, 0.000000000000000000, -3.343241100358131282E-16 ) ) ;
#9471 = CARTESIAN_POINT ( 'NONE',  ( 0.000000000000000000, 0.000000000000000000, -5.000000000000000000 ) ) ;
#9472 = VERTEX_POINT ( 'NONE', #921 ) ;
#9473 =( NAMED_UNIT ( * ) SI_UNIT ( $, .STERADIAN. ) SOLID_ANGLE_UNIT ( ) );
#9474 = ORIENTED_EDGE ( 'NONE', *, *, #14762, .F. ) ;
#9475 = MANIFOLD_SOLID_BREP ( 'CirPattern1', #12026 ) ;
#9476 = DIRECTION ( 'NONE',  ( 0.8660254037844387076, 0.000000000000000000, -0.4999999999999997224 ) ) ;
#9477 = ORIENTED_EDGE ( 'NONE', *, *, #11766, .F. ) ;
#9478 = EDGE_CURVE ( 'NONE', #5642, #5349, #3578, .T. ) ;
#9479 = AXIS2_PLACEMENT_3D ( 'NONE', #3501, #9730, #8379 ) ;
#9480 = EDGE_CURVE ( 'NONE', #2808, #14971, #14981, .T. ) ;
#9481 = DIRECTION ( 'NONE',  ( 0.000000000000000000, 1.224646799147353207E-16, 1.000000000000000000 ) ) ;
#9482 = DIRECTION ( 'NONE',  ( -1.000000000000000000, 0.000000000000000000, 0.000000000000000000 ) ) ;
#9483 = CARTESIAN_POINT ( 'NONE',  ( 3.753672977998667726, 3.033343224707664376, -0.2499999986344070280 ) ) ;
#9484 = DIRECTION ( 'NONE',  ( 0.5000000000000041078, 0.000000000000000000, -0.8660254037844364872 ) ) ;
#9485 = CARTESIAN_POINT ( 'NONE',  ( -4.276409079477644148, -1.261996585732578335, -0.06249999863440838799 ) ) ;
#9486 = CARTESIAN_POINT ( 'NONE',  ( 4.209348295687701302, 3.401574460001766109, -0.9375000000000017764 ) ) ;
#9487 = CIRCLE ( 'NONE', #466, 2.000000000000000888 ) ;
#9488 = CARTESIAN_POINT ( 'NONE',  ( -19.99999999999956657, -9.000000000000001776, -2.499999999999120259 ) ) ;
#9489 = ORIENTED_EDGE ( 'NONE', *, *, #5610, .F. ) ;
#9490 = CARTESIAN_POINT ( 'NONE',  ( 4.631580223510930239, 1.444531747605005878E-11, -0.2579703047231843294 ) ) ;
#9491 = LINE ( 'NONE', #617, #13840 ) ;
#9492 = CARTESIAN_POINT ( 'NONE',  ( 0.000000000000000000, -32.00000000000000000, 0.000000000000000000 ) ) ;
#9493 = ORIENTED_EDGE ( 'NONE', *, *, #11599, .F. ) ;
#9494 = CARTESIAN_POINT ( 'NONE',  ( -19.99999999999956657, -9.000000000000001776, 8.786575603324269439E-13 ) ) ;
#9495 = ORIENTED_EDGE ( 'NONE', *, *, #6505, .T. ) ;
#9496 = CIRCLE ( 'NONE', #11799, 2.499999999999998668 ) ;
#9497 = ORIENTED_EDGE ( 'NONE', *, *, #4144, .T. ) ;
#9498 = CARTESIAN_POINT ( 'NONE',  ( -0.5093500532425060401, -4.799145180956616130, -0.8749999986344056957 ) ) ;
#9499 = ADVANCED_FACE ( 'NONE', ( #1226 ), #3817, .T. ) ;
#9500 = CARTESIAN_POINT ( 'NONE',  ( -90.00000000000000000, -35.00000000000000711, -7.500000000000000000 ) ) ;
#9501 = EDGE_CURVE ( 'NONE', #5431, #1476, #9877, .T. ) ;
#9502 = ADVANCED_FACE ( 'NONE', ( #6416 ), #13741, .T. ) ;
#9503 = CARTESIAN_POINT ( 'NONE',  ( -34.99999999999999289, -13.00000000000000178, -1.999999999999170441 ) ) ;
#9504 = CARTESIAN_POINT ( 'NONE',  ( -39.99999999999999289, -13.00000000000000178, 8.300651832549021947E-13 ) ) ;
#9505 = CARTESIAN_POINT ( 'NONE',  ( 47.32050807568875683, -37.00000000000000711, 41.96152422706633445 ) ) ;
#9506 = AXIS2_PLACEMENT_3D ( 'NONE', #5908, #13642, #12028 ) ;
#9507 = CARTESIAN_POINT ( 'NONE',  ( 0.5711823568785989735, 5.381735091635026613, -7.812500000000005329 ) ) ;
#9508 = CARTESIAN_POINT ( 'NONE',  ( 5.000000000000004441, -2.247904837838113790E-16, -3.045263047592945860 ) ) ;
#9509 = CARTESIAN_POINT ( 'NONE',  ( 1.846868145590736310, -30.87500000136559564, 4.458734124999997661 ) ) ;
#9510 = CARTESIAN_POINT ( 'NONE',  ( 4.276409079477644148, 1.261996585732577891, -0.3124999986344085823 ) ) ;
#9511 = ORIENTED_EDGE ( 'NONE', *, *, #14327, .T. ) ;
#9512 = CARTESIAN_POINT ( 'NONE',  ( 2.411464220262452773, 7.267994521134256480, -7.491772860716523041 ) ) ;
#9513 = ORIENTED_EDGE ( 'NONE', *, *, #11222, .T. ) ;
#9514 = CIRCLE ( 'NONE', #8752, 2.649999999999985700 ) ;
#9515 = ORIENTED_EDGE ( 'NONE', *, *, #7862, .F. ) ;
#9516 = VECTOR ( 'NONE', #768, 1000.000000000000000 ) ;
#9517 = VERTEX_POINT ( 'NONE', #12528 ) ;
#9518 = PRODUCT ( 'Synchronized Concentric Jaws', 'Synchronized Concentric Jaws', '', ( #2592 ) ) ;
#9519 = CARTESIAN_POINT ( 'NONE',  ( 4.458734124999999437, -26.75000000136559564, 1.846868145590737864 ) ) ;
#9520 = CARTESIAN_POINT ( 'NONE',  ( 3.061616997868383141E-16, -23.87500000273118772, -5.000000000000000000 ) ) ;
#9521 = EDGE_CURVE ( 'NONE', #10516, #12023, #10024, .T. ) ;
#9522 = AXIS2_PLACEMENT_3D ( 'NONE', #15390, #6988, #1879 ) ;
#9523 = CARTESIAN_POINT ( 'NONE',  ( -6.762176242291807225E-13, 40.00000000000000000, 64.84999999999932641 ) ) ;
#9524 = DIRECTION ( 'NONE',  ( 0.5000000000000003331, -6.505213034913029562E-16, 0.8660254037844385966 ) ) ;
#9525 = CARTESIAN_POINT ( 'NONE',  ( 2.548804901056335857E-15, 4.736522675502163437, -3.681124513963624612 ) ) ;
#9526 = CONICAL_SURFACE ( 'NONE', #11578, 7.500000000000001776, 0.8594454914424796144 ) ;
#9527 = CARTESIAN_POINT ( 'NONE',  ( -5.000000000000000888, -23.56250000000000000, -2.071067811865475949 ) ) ;
#9528 = CARTESIAN_POINT ( 'NONE',  ( 0.5093500532425063732, 4.799145180956616130, -6.124999998634407916 ) ) ;
#9529 = CARTESIAN_POINT ( 'NONE',  ( -21.01110699893041556, 2.000000000000000000, -36.39230484541334221 ) ) ;
#9530 = CARTESIAN_POINT ( 'NONE',  ( -4.524602526901894350, -1.321206833522081014, -0.2058151098866615736 ) ) ;
#9531 = CARTESIAN_POINT ( 'NONE',  ( 5.000000000000000000, -22.12500000273118417, 0.000000000000000000 ) ) ;
#9532 = VERTEX_POINT ( 'NONE', #2674 ) ;
#9533 = DIRECTION ( 'NONE',  ( 1.000000000000000000, 0.000000000000000000, 0.000000000000000000 ) ) ;
#9534 = ADVANCED_FACE ( 'NONE', ( #10050 ), #14809, .T. ) ;
#9535 = CARTESIAN_POINT ( 'NONE',  ( 5.200000000000002842, 0.000000000000000000, 0.000000000000000000 ) ) ;
#9536 = ORIENTED_EDGE ( 'NONE', *, *, #6817, .T. ) ;
#9537 = ORIENTED_EDGE ( 'NONE', *, *, #11221, .T. ) ;
#9538 = CARTESIAN_POINT ( 'NONE',  ( -7.897827455343219505, -1.533134349199730018, -7.633632140068247196 ) ) ;
#9539 = CARTESIAN_POINT ( 'NONE',  ( -3.152801135295367985, -27.81250000136559564, 3.152801135295367096 ) ) ;
#9540 = DIRECTION ( 'NONE',  ( 0.000000000000000000, 0.000000000000000000, 1.000000000000000000 ) ) ;
#9541 = ORIENTED_EDGE ( 'NONE', *, *, #12871, .F. ) ;
#9543 = AXIS2_PLACEMENT_3D ( 'NONE', #2055, #8135, #12954 ) ;
#9542 = LINE ( 'NONE', #5818, #6057 ) ;
#9544 = DIRECTION ( 'NONE',  ( 0.000000000000000000, 0.000000000000000000, -1.000000000000000000 ) ) ;
#9545 = DIRECTION ( 'NONE',  ( 0.000000000000000000, 1.000000000000000000, 0.000000000000000000 ) ) ;
#9546 = CARTESIAN_POINT ( 'NONE',  ( 3.152801135295366208, -23.81250000136559564, 3.152801135295367985 ) ) ;
#9547 = CARTESIAN_POINT ( 'NONE',  ( 0.000000000000000000, 20.00000000000000000, 0.000000000000000000 ) ) ;
#9548 = DIRECTION ( 'NONE',  ( -1.000000000000000000, 2.602085213965212219E-15, 0.000000000000000000 ) ) ;
#9549 = FACE_OUTER_BOUND ( 'NONE', #6539, .T. ) ;
#9550 = CYLINDRICAL_SURFACE ( 'NONE', #10017, 2.100000000000000089 ) ;
#9551 = EDGE_CURVE ( 'NONE', #1675, #2479, #11334, .T. ) ;
#9553 = EDGE_CURVE ( 'NONE', #11169, #6761, #282, .T. ) ;
#9552 = EDGE_LOOP ( 'NONE', ( #1871, #622, #9764 ) ) ;
#9554 = ORIENTED_EDGE ( 'NONE', *, *, #1540, .F. ) ;
#9555 = CARTESIAN_POINT ( 'NONE',  ( -4.000000000000000000, 0.9868501483902560878, -0.09357334158579519445 ) ) ;
#9556 = ORIENTED_EDGE ( 'NONE', *, *, #7348, .F. ) ;
#9557 = DIRECTION ( 'NONE',  ( 0.000000000000000000, 1.000000000000000000, 0.000000000000000000 ) ) ;
#9558 =( BOUNDED_CURVE ( )  B_SPLINE_CURVE ( 2, ( #14400, #10530, #6893, #4300, #11797, #15465, #750, #8034, #12928, #15615, #5675 ),
 .UNSPECIFIED., .F., .F. ) 
 B_SPLINE_CURVE_WITH_KNOTS ( ( 3, 2, 2, 2, 2, 3 ),
 ( 0.6045872658012773071, 0.6125000000000000444, 0.6250000000000000000, 0.6374999999999999556, 0.6500000000000000222, 0.6545872658012773515 ),
 .UNSPECIFIED. ) 
 CURVE ( )  GEOMETRIC_REPRESENTATION_ITEM ( )  RATIONAL_B_SPLINE_CURVE ( ( 0.9646335149384808183, 0.9518143178943441196, 1.000000000000000000, 0.9238795325112867385, 1.000000000000000000, 0.9238795325112867385, 1.000000000000000000, 0.9238795325112867385, 1.000000000000000000, 0.9720652146169423968, 0.9646335149384803742 ) ) 
 REPRESENTATION_ITEM ( '' )  );
#9559 = CARTESIAN_POINT ( 'NONE',  ( 3.401574460001763445, -4.209348295687703079, -3.062499997268815388 ) ) ;
#9560 = DIRECTION ( 'NONE',  ( -0.5000000000000041078, 0.000000000000000000, 0.8660254037844364872 ) ) ;
#9561 = CARTESIAN_POINT ( 'NONE',  ( -0.5093500532425060401, -4.799145180956616130, -2.874999998634407472 ) ) ;
#9562 = LINE ( 'NONE', #8365, #12313 ) ;
#9563 = FILL_AREA_STYLE ('',( #11016 ) ) ;
#9564 = EDGE_CURVE ( 'NONE', #6730, #2868, #10125, .T. ) ;
#9565 = ORIENTED_EDGE ( 'NONE', *, *, #1278, .T. ) ;
#9566 = CARTESIAN_POINT ( 'NONE',  ( -2.071067811865503483, -22.68750000000000000, -4.999999999999971578 ) ) ;
#9567 = ORIENTED_EDGE ( 'NONE', *, *, #10365, .F. ) ;
#9568 = CARTESIAN_POINT ( 'NONE',  ( 5.000000000000000000, -32.00000000000000000, 0.000000000000000000 ) ) ;
#9569 = VERTEX_POINT ( 'NONE', #15056 ) ;
#9570 = VERTEX_POINT ( 'NONE', #13489 ) ;
#9571 = CARTESIAN_POINT ( 'NONE',  ( 30.02221399786052913, 88.59290746114278647, 16.00000000000001066 ) ) ;
#9572 = DIRECTION ( 'NONE',  ( 0.000000000000000000, 1.000000000000000000, 0.000000000000000000 ) ) ;
#9573 = CARTESIAN_POINT ( 'NONE',  ( -115.0000000000000142, -10.00000000000000888, 17.50000000000000000 ) ) ;
#9574 = DIRECTION ( 'NONE',  ( 0.000000000000000000, 0.000000000000000000, 1.000000000000000000 ) ) ;
#9575 = CARTESIAN_POINT ( 'NONE',  ( 6.000000000000000000, -20.00000000000000000, 1.500000000000000000 ) ) ;
#9576 = CARTESIAN_POINT ( 'NONE',  ( -2.390265326283148806, -4.391654775818394363, -1.249999997268814278 ) ) ;
#9577 = LINE ( 'NONE', #15890, #497 ) ;
#9578 = EDGE_CURVE ( 'NONE', #2190, #1108, #15657, .T. ) ;
#9579 = CARTESIAN_POINT ( 'NONE',  ( 17.00000000000000000, 0.000000000000000000, 0.000000000000000000 ) ) ;
#9580 = CARTESIAN_POINT ( 'NONE',  ( -4.458734124999999437, -31.25000000136559564, -1.846868145590735644 ) ) ;
#9581 = ADVANCED_FACE ( 'NONE', ( #12449 ), #1386, .T. ) ;
#9582 = CARTESIAN_POINT ( 'NONE',  ( 3.916244202832140253, -2.131511515620588160, 1.562500001365592972 ) ) ;
#9583 = ORIENTED_EDGE ( 'NONE', *, *, #13822, .F. ) ;
#9584 = CARTESIAN_POINT ( 'NONE',  ( 35.00000000000000000, 37.00000000000000000, -8.572527594031472993E-15 ) ) ;
#9585 = ORIENTED_EDGE ( 'NONE', *, *, #3562, .T. ) ;
#9586 = ORIENTED_EDGE ( 'NONE', *, *, #3512, .F. ) ;
#9587 = ORIENTED_EDGE ( 'NONE', *, *, #13550, .T. ) ;
#9588 = CARTESIAN_POINT ( 'NONE',  ( 3.152801135295367541, -28.56250000136559564, -3.152801135295367541 ) ) ;
#9589 = DIRECTION ( 'NONE',  ( 0.000000000000000000, 0.000000000000000000, 1.000000000000000000 ) ) ;
#9590 = CARTESIAN_POINT ( 'NONE',  ( 3.061616997868383141E-16, -29.87500000273118417, -5.000000000000000000 ) ) ;
#9591 = DIRECTION ( 'NONE',  ( -0.000000000000000000, 1.000000000000000000, -0.000000000000000000 ) ) ;
#9592 = DIRECTION ( 'NONE',  ( 0.000000000000000000, 0.000000000000000000, -1.000000000000000000 ) ) ;
#9593 = CARTESIAN_POINT ( 'NONE',  ( 3.535533905932738197, -23.87500000000000000, -3.535533905932738197 ) ) ;
#9594 = CARTESIAN_POINT ( 'NONE',  ( -5.381735091635034607, 0.5711823568785950878, -1.562500000000000666 ) ) ;
#9595 = CARTESIAN_POINT ( 'NONE',  ( 4.795541693661363958, 1.415196051561583790, -8.437499998634409692 ) ) ;
#9596 = CARTESIAN_POINT ( 'NONE',  ( 23.49999999999956657, -8.782289339527253835E-13, 1.500000000000000000 ) ) ;
#9597 = CARTESIAN_POINT ( 'NONE',  ( -4.458734125000000326, -31.00000000136559564, -1.846868145590735644 ) ) ;
#9598 = EDGE_CURVE ( 'NONE', #8804, #6, #1120, .T. ) ;
#9599 = VERTEX_POINT ( 'NONE', #8423 ) ;
#9600 = DIRECTION ( 'NONE',  ( 0.000000000000000000, 0.000000000000000000, 1.000000000000000000 ) ) ;
#9601 = ORIENTED_EDGE ( 'NONE', *, *, #8323, .F. ) ;
#9602 = ORIENTED_EDGE ( 'NONE', *, *, #22, .T. ) ;
#9603 = CARTESIAN_POINT ( 'NONE',  ( 42.02221399786069611, 0.000000000000000000, 1.040834085586084257E-13 ) ) ;
#9604 = CARTESIAN_POINT ( 'NONE',  ( 4.458734124999999437, -27.43750000136559564, 0.000000000000000000 ) ) ;
#9605 = CARTESIAN_POINT ( 'NONE',  ( 0.000000000000000000, 2.357898499370433054, -1.951563910473907981E-15 ) ) ;
#9606 = ORIENTED_EDGE ( 'NONE', *, *, #6863, .F. ) ;
#9607 = CYLINDRICAL_SURFACE ( 'NONE', #2202, 2.649999999999992806 ) ;
#9608 = AXIS2_PLACEMENT_3D ( 'NONE', #3447, #12163, #14527 ) ;
#9609 = CYLINDRICAL_SURFACE ( 'NONE', #11074, 2.649999999999999467 ) ;
#9610 = CARTESIAN_POINT ( 'NONE',  ( -1.828356344711647319, -3.563200125723192002, -1.076197711133951296E-14 ) ) ;
#9611 = DIRECTION ( 'NONE',  ( -1.000000000000000000, -1.239088197126290324E-16, 0.000000000000000000 ) ) ;
#9612 = CARTESIAN_POINT ( 'NONE',  ( -8.190561711645485556E-16, -24.93750000136559564, 4.458734124999999437 ) ) ;
#9613 = DIRECTION ( 'NONE',  ( 0.000000000000000000, 0.000000000000000000, -1.000000000000000000 ) ) ;
#9614 = FACE_OUTER_BOUND ( 'NONE', #13172, .T. ) ;
#9615 = CARTESIAN_POINT ( 'NONE',  ( -28.86751345948130165, -37.00000000000000711, 20.00000000000000355 ) ) ;
#9616 = CIRCLE ( 'NONE', #2124, 25.00000000000000000 ) ;
#9617 = DIRECTION ( 'NONE',  ( 0.000000000000000000, -1.000000000000000000, 0.000000000000000000 ) ) ;
#9618 = VECTOR ( 'NONE', #1533, 1000.000000000000000 ) ;
#9619 = EDGE_LOOP ( 'NONE', ( #14739, #1829 ) ) ;
#9620 =( LENGTH_UNIT ( ) NAMED_UNIT ( * ) SI_UNIT ( .MILLI., .METRE. ) );
#9621 = ORIENTED_EDGE ( 'NONE', *, *, #4689, .T. ) ;
#9622 = CARTESIAN_POINT ( 'NONE',  ( 3.679171394226031122, 2.494631558665830973, -0.3503314178412474389 ) ) ;
#9623 = EDGE_LOOP ( 'NONE', ( #159, #1813, #12038, #5786 ) ) ;
#9624 = VECTOR ( 'NONE', #6607, 1000.000000000000000 ) ;
#9625 = DIRECTION ( 'NONE',  ( -0.000000000000000000, -1.000000000000000000, -0.000000000000000000 ) ) ;
#9626 = EDGE_CURVE ( 'NONE', #13586, #2123, #10181, .T. ) ;
#9627 = CARTESIAN_POINT ( 'NONE',  ( -3.033343224707664376, 3.753672977998667726, 1.000000001365594082 ) ) ;
#9628 = DIRECTION ( 'NONE',  ( 1.000000000000000000, -6.123233995736766036E-17, -6.123233995736764803E-17 ) ) ;
#9629 = PRODUCT ( 'BR-003', 'BR-003', '', ( #15545 ) ) ;
#9631 = VECTOR ( 'NONE', #9351, 1000.000000000000000 ) ;
#9630 = CARTESIAN_POINT ( 'NONE',  ( -4.799145180956616130, 0.5093500532425063732, -1.124999998634405918 ) ) ;
#9632 = FACE_OUTER_BOUND ( 'NONE', #9398, .T. ) ;
#9633 = DIRECTION ( 'NONE',  ( 0.000000000000000000, 1.000000000000000000, 0.000000000000000000 ) ) ;
#9634 = VERTEX_POINT ( 'NONE', #15773 ) ;
#9635 = CARTESIAN_POINT ( 'NONE',  ( -3.535533905932738641, -22.37500000000000000, 3.535533905932737309 ) ) ;
#9636 = EDGE_LOOP ( 'NONE', ( #15767, #1595, #9244, #14153 ) ) ;
#9637 = FACE_OUTER_BOUND ( 'NONE', #15962, .T. ) ;
#9638 = CARTESIAN_POINT ( 'NONE',  ( -91.33974596215560382, -110.0591436588189396, -7.500000000000000000 ) ) ;
#9639 = VERTEX_POINT ( 'NONE', #10756 ) ;
#9640 = CARTESIAN_POINT ( 'NONE',  ( 3.753672977998667726, 3.033343224707664820, -3.499999998634409692 ) ) ;
#9641 =( BOUNDED_CURVE ( )  B_SPLINE_CURVE ( 2, ( #13081, #3231, #3317, #15368, #4376, #13160, #8024, #8267, #8179, #11868, #9309 ),
 .UNSPECIFIED., .F., .F. ) 
 B_SPLINE_CURVE_WITH_KNOTS ( ( 3, 2, 2, 2, 2, 3 ),
 ( 0.4545872658012772849, 0.4625000000000000222, 0.4749999999999999778, 0.4874999999999999889, 0.5000000000000000000, 0.5045872658012773293 ),
 .UNSPECIFIED. ) 
 CURVE ( )  GEOMETRIC_REPRESENTATION_ITEM ( )  RATIONAL_B_SPLINE_CURVE ( ( 0.9646335149384808183, 0.9518143178943437865, 1.000000000000000000, 0.9238795325112867385, 1.000000000000000000, 0.9238795325112867385, 1.000000000000000000, 0.9238795325112867385, 1.000000000000000000, 0.9720652146169423968, 0.9646335149384803742 ) ) 
 REPRESENTATION_ITEM ( '' )  );
#9642 = DIRECTION ( 'NONE',  ( -0.4999999999999997780, 0.000000000000000000, -0.8660254037844388186 ) ) ;
#9643 = ADVANCED_FACE ( 'NONE', ( #14471, #13396 ), #14628, .T. ) ;
#9644 = EDGE_CURVE ( 'NONE', #15708, #14775, #13753, .T. ) ;
#9645 = FACE_OUTER_BOUND ( 'NONE', #2924, .T. ) ;
#9646 = CARTESIAN_POINT ( 'NONE',  ( -4.209348295687703079, -3.401574460001763445, -2.437500000000003109 ) ) ;
#9647 = CARTESIAN_POINT ( 'NONE',  ( -28.86751345948130165, 88.59290746114278647, 18.00000000000000355 ) ) ;
#9648 = PRESENTATION_LAYER_ASSIGNMENT (  '', '', ( #8382 ) ) ;
#9649 = CARTESIAN_POINT ( 'NONE',  ( 5.381735091635035495, -0.5711823568785978633, 1.062500002731182613 ) ) ;
#9650 = CARTESIAN_POINT ( 'NONE',  ( -124.9999999999999858, -115.2072594216369907, 7.500000000000001776 ) ) ;
#9651 = CARTESIAN_POINT ( 'NONE',  ( 2.730187237215162345E-16, -24.43750000136559564, -4.458734124999999437 ) ) ;
#9652 = AXIS2_PLACEMENT_3D ( 'NONE', #14865, #14780, #3704 ) ;
#9653 = CARTESIAN_POINT ( 'NONE',  ( 3.916244202832140253, -2.131511515620588160, -5.437499998634406140 ) ) ;
#9654 = ORIENTED_EDGE ( 'NONE', *, *, #6405, .F. ) ;
#9655 = DIRECTION ( 'NONE',  ( -0.000000000000000000, -1.000000000000000000, -0.000000000000000000 ) ) ;
#9656 = VERTEX_POINT ( 'NONE', #10987 ) ;
#9657 = ORIENTED_EDGE ( 'NONE', *, *, #14261, .T. ) ;
#9658 = ORIENTED_EDGE ( 'NONE', *, *, #656, .T. ) ;
#9659 = DIRECTION ( 'NONE',  ( -0.4999999999999997224, 0.000000000000000000, -0.8660254037844388186 ) ) ;
#9660 = DIRECTION ( 'NONE',  ( 0.000000000000000000, 0.000000000000000000, -1.000000000000000000 ) ) ;
#9661 = AXIS2_PLACEMENT_3D ( 'NONE', #14416, #7146, #9484 ) ;
#9662 = CARTESIAN_POINT ( 'NONE',  ( 2.071067811865485275, -30.31250000273118062, 4.999999999999989342 ) ) ;
#9663 = EDGE_CURVE ( 'NONE', #6965, #9656, #4866, .T. ) ;
#9664 = EDGE_CURVE ( 'NONE', #7472, #2457, #6164, .T. ) ;
#9665 = AXIS2_PLACEMENT_3D ( 'NONE', #15254, #311, #11284 ) ;
#9666 = DIRECTION ( 'NONE',  ( -0.000000000000000000, 1.000000000000000000, -0.000000000000000000 ) ) ;
#9667 = FACE_BOUND ( 'NONE', #1194, .T. ) ;
#9668 = DIRECTION ( 'NONE',  ( 1.000000000000000000, 0.000000000000000000, 0.000000000000000000 ) ) ;
#9669 = CARTESIAN_POINT ( 'NONE',  ( -2.390265326283148806, -4.391654775818394363, -1.375000000000001332 ) ) ;
#9670 = DIRECTION ( 'NONE',  ( 0.000000000000000000, 0.000000000000000000, -1.000000000000000000 ) ) ;
#9671 = CARTESIAN_POINT ( 'NONE',  ( 3.187317364896726790, -3.801046099509943765, -0.03262248246693635195 ) ) ;
#9672 = CARTESIAN_POINT ( 'NONE',  ( 3.152801135295367541, -30.31250000136559564, -3.152801135295367541 ) ) ;
#9673 =( GEOMETRIC_REPRESENTATION_CONTEXT ( 3 ) GLOBAL_UNCERTAINTY_ASSIGNED_CONTEXT ( ( #4961 ) ) GLOBAL_UNIT_ASSIGNED_CONTEXT ( ( #4539, #4305, #8196 ) ) REPRESENTATION_CONTEXT ( 'NONE', 'WORKASPACE' ) );
#9674 = CARTESIAN_POINT ( 'NONE',  ( 4.799145180956616130, -0.5093500532425063732, -1.624999998634406362 ) ) ;
#9675 = ORIENTED_EDGE ( 'NONE', *, *, #12013, .F. ) ;
#9676 = VECTOR ( 'NONE', #11733, 1000.000000000000000 ) ;
#9677 = DIRECTION ( 'NONE',  ( 0.000000000000000000, 0.000000000000000000, 1.000000000000000000 ) ) ;
#9678 = VERTEX_POINT ( 'NONE', #8576 ) ;
#9679 = ORIENTED_EDGE ( 'NONE', *, *, #8343, .F. ) ;
#9680 = FACE_OUTER_BOUND ( 'NONE', #1460, .T. ) ;
#9681 = CARTESIAN_POINT ( 'NONE',  ( -1.846868145590734756, -30.12500000136559208, -4.458734125000000326 ) ) ;
#9682 = CARTESIAN_POINT ( 'NONE',  ( 0.000000000000000000, -13.00000000000000178, 0.000000000000000000 ) ) ;
#9683 = ORIENTED_EDGE ( 'NONE', *, *, #2620, .F. ) ;
#9684 = DIRECTION ( 'NONE',  ( -0.000000000000000000, 1.000000000000000000, -0.000000000000000000 ) ) ;
#9685 = ADVANCED_FACE ( 'NONE', ( #899 ), #13465, .T. ) ;
#9686 = EDGE_CURVE ( 'NONE', #15795, #11117, #7279, .T. ) ;
#9687 = CIRCLE ( 'NONE', #4789, 7.500000000000001776 ) ;
#9688 = CARTESIAN_POINT ( 'NONE',  ( 2.602085213965210642E-15, 8.660254037844392627, -1.000000000000000888 ) ) ;
#9689 = CARTESIAN_POINT ( 'NONE',  ( -0.3198814748697807464, -4.434118497892185040, -0.3507732604232532969 ) ) ;
#9690 = DIRECTION ( 'NONE',  ( 0.000000000000000000, 0.000000000000000000, -1.000000000000000000 ) ) ;
#9691 = AXIS2_PLACEMENT_3D ( 'NONE', #3232, #15688, #14154 ) ;
#9692 = CARTESIAN_POINT ( 'NONE',  ( -1.846868145590737420, -22.00000000136559208, 4.458734124999999437 ) ) ;
#9693 = CIRCLE ( 'NONE', #2724, 10.12668159690567649 ) ;
#9694 = CARTESIAN_POINT ( 'NONE',  ( -1.908195823574487804E-14, -8.660254037844392627, -1.000000000000000888 ) ) ;
#9695 =( REPRESENTATION_RELATIONSHIP ('NONE','NONE', #4176, #3049 ) REPRESENTATION_RELATIONSHIP_WITH_TRANSFORMATION ( #10443 )SHAPE_REPRESENTATION_RELATIONSHIP( ) );
#9696 = CARTESIAN_POINT ( 'NONE',  ( -5.000000000000004441, -7.530481206757679743E-15, -1.420263044861758361 ) ) ;
#9697 = DIRECTION ( 'NONE',  ( 0.000000000000000000, 0.000000000000000000, -1.000000000000000000 ) ) ;
#9698 = PLANE ( 'NONE',  #15437 ) ;
#9699 = DIRECTION ( 'NONE',  ( 0.000000000000000000, 0.000000000000000000, 1.000000000000000000 ) ) ;
#9700 = ORIENTED_EDGE ( 'NONE', *, *, #15417, .F. ) ;
#9701 = VECTOR ( 'NONE', #1992, 1000.000000000000000 ) ;
#9702 = SURFACE_SIDE_STYLE ('',( #23 ) ) ;
#9703 = VERTEX_POINT ( 'NONE', #8 ) ;
#9704 = FACE_OUTER_BOUND ( 'NONE', #10724, .T. ) ;
#9705 = VECTOR ( 'NONE', #3136, 1000.000000000000000 ) ;
#9706 = EDGE_LOOP ( 'NONE', ( #7431, #14282, #11154, #3103 ) ) ;
#9707 = ADVANCED_FACE ( 'NONE', ( #4610 ), #4684, .F. ) ;
#9708 = DIRECTION ( 'NONE',  ( 0.000000000000000000, 0.000000000000000000, 1.000000000000000000 ) ) ;
#9709 = CIRCLE ( 'NONE', #2744, 2.041999999999999815 ) ;
#9710 = CARTESIAN_POINT ( 'NONE',  ( -5.000000000000000888, -25.56250000273118417, 2.071067811865474617 ) ) ;
#9711 = CARTESIAN_POINT ( 'NONE',  ( -2.131511515620587272, -3.916244202832140253, -1.687499998634406362 ) ) ;
#9712 = DIRECTION ( 'NONE',  ( 0.000000000000000000, 0.000000000000000000, 1.000000000000000000 ) ) ;
#9713 = AXIS2_PLACEMENT_3D ( 'NONE', #624, #9421, #778 ) ;
#9714 = CARTESIAN_POINT ( 'NONE',  ( -3.753672977998669946, -3.033343224707661712, 1.365593156898739876E-09 ) ) ;
#9715 = DIRECTION ( 'NONE',  ( 1.000000000000000000, 0.000000000000000000, 0.000000000000000000 ) ) ;
#9716 = CARTESIAN_POINT ( 'NONE',  ( 3.750000000000004441, -6.495190528383289141, 0.000000000000000000 ) ) ;
#9717 = ORIENTED_EDGE ( 'NONE', *, *, #3962, .T. ) ;
#9718 = CARTESIAN_POINT ( 'NONE',  ( -9.184850993605147944E-16, -21.37500000273118772, 5.000000000000000000 ) ) ;
#9719 =( NAMED_UNIT ( * ) PLANE_ANGLE_UNIT ( ) SI_UNIT ( $, .RADIAN. ) );
#9720 = ADVANCED_FACE ( 'NONE', ( #2403 ), #9609, .F. ) ;
#9721 = VERTEX_POINT ( 'NONE', #1047 ) ;
#9722 = FACE_OUTER_BOUND ( 'NONE', #14124, .T. ) ;
#9723 = LINE ( 'NONE', #6092, #14627 ) ;
#9724 = ORIENTED_EDGE ( 'NONE', *, *, #10590, .T. ) ;
#9725 = ORIENTED_EDGE ( 'NONE', *, *, #15783, .T. ) ;
#9726 = CARTESIAN_POINT ( 'NONE',  ( -3.033343224707664820, 3.753672977998667726, -1.249999998634407916 ) ) ;
#9727 = EDGE_CURVE ( 'NONE', #10564, #3510, #11226, .T. ) ;
#9728 = DIRECTION ( 'NONE',  ( 0.000000000000000000, 0.000000000000000000, 1.000000000000000000 ) ) ;
#9729 = CARTESIAN_POINT ( 'NONE',  ( 5.384454397937118664, 0.000000000000000000, -4.484454397937119197 ) ) ;
#9730 = DIRECTION ( 'NONE',  ( 0.000000000000000000, 0.000000000000000000, 1.000000000000000000 ) ) ;
#9732 = CARTESIAN_POINT ( 'NONE',  ( -39.99999999999999289, -9.000000000000001776, 8.300651832549021947E-13 ) ) ;
#9731 = AXIS2_PLACEMENT_3D ( 'NONE', #13926, #8690, #3906 ) ;
#9733 = FACE_BOUND ( 'NONE', #3233, .T. ) ;
#9734 = CARTESIAN_POINT ( 'NONE',  ( 4.209348295687701302, 3.401574460001765665, 0.1875000027311836681 ) ) ;
#9735 = CARTESIAN_POINT ( 'NONE',  ( -5.000000000000000888, -22.56250000273118772, 2.071067811865474617 ) ) ;
#9736 = CARTESIAN_POINT ( 'NONE',  ( -4.458734124999999437, -25.25000000136559564, -1.846868145590735644 ) ) ;
#9737 = CARTESIAN_POINT ( 'NONE',  ( 0.5093500532425063732, 4.799145180956616130, -5.124999998634405252 ) ) ;
#9738 = VECTOR ( 'NONE', #11272, 1000.000000000000000 ) ;
#9739 = DIRECTION ( 'NONE',  ( 0.000000000000000000, 1.000000000000000000, 0.000000000000000000 ) ) ;
#9740 = EDGE_CURVE ( 'NONE', #2783, #2143, #10039, .T. ) ;
#9741 = ORIENTED_EDGE ( 'NONE', *, *, #13823, .F. ) ;
#9742 = ORIENTED_EDGE ( 'NONE', *, *, #2412, .T. ) ;
#9743 = ADVANCED_FACE ( 'NONE', ( #13165 ), #3544, .F. ) ;
#9744 =( BOUNDED_CURVE ( )  B_SPLINE_CURVE ( 2, ( #532, #7806, #13999, #5369, #13842, #12698, #1641, #11344, #210, #5450, #2926 ),
 .UNSPECIFIED., .F., .T. ) 
 B_SPLINE_CURVE_WITH_KNOTS ( ( 3, 2, 2, 2, 2, 3 ),
 ( 0.6045872658012773071, 0.6125000000000000444, 0.6250000000000000000, 0.6374999999999999556, 0.6500000000000000222, 0.6545872658012773515 ),
 .UNSPECIFIED. ) 
 CURVE ( )  GEOMETRIC_REPRESENTATION_ITEM ( )  RATIONAL_B_SPLINE_CURVE ( ( 0.9646335149384808183, 0.9518143178943441196, 1.000000000000000000, 0.9238795325112867385, 1.000000000000000000, 0.9238795325112867385, 1.000000000000000000, 0.9238795325112867385, 1.000000000000000000, 0.9720652146169423968, 0.9646335149384803742 ) ) 
 REPRESENTATION_ITEM ( '' )  );
#9745 = SHAPE_REPRESENTATION_RELATIONSHIP ( 'NONE' , 'NONE' ,  #4696, #14078 ) ;
#9746 = ORIENTED_EDGE ( 'NONE', *, *, #13573, .F. ) ;
#9747 = CARTESIAN_POINT ( 'NONE',  ( -4.458734125000001214, -22.12500000136559564, 1.846868145590734089 ) ) ;
#9748 = AXIS2_PLACEMENT_3D ( 'NONE', #11623, #5494, #4279 ) ;
#9749 = CARTESIAN_POINT ( 'NONE',  ( -1.154700538379406893, 0.000000000000000000, -34.00000000000000711 ) ) ;
#9750 = CARTESIAN_POINT ( 'NONE',  ( 2.500000000000000000, 2.357898499370433054, -1.951563910473907981E-15 ) ) ;
#9751 = VECTOR ( 'NONE', #9805, 1000.000000000000000 ) ;
#9752 = CARTESIAN_POINT ( 'NONE',  ( 7.500000000000000000, 4.330127018922190096, -9.999999999999998224 ) ) ;
#9753 = DIRECTION ( 'NONE',  ( -4.336808689942013792E-16, 0.000000000000000000, 1.000000000000000000 ) ) ;
#9754 = CYLINDRICAL_SURFACE ( 'NONE', #15474, 5.000000000000000888 ) ;
#9755 = CARTESIAN_POINT ( 'NONE',  ( 3.401574460001763001, -4.209348295687703967, -2.187500000000002665 ) ) ;
#9756 = DIRECTION ( 'NONE',  ( -0.000000000000000000, -0.000000000000000000, 1.000000000000000000 ) ) ;
#9757 = CONICAL_SURFACE ( 'NONE', #3563, 4.000000000000000000, 0.8911886515913786111 ) ;
#9758 = DIRECTION ( 'NONE',  ( -0.000000000000000000, -1.000000000000000000, -0.000000000000000000 ) ) ;
#9759 = CARTESIAN_POINT ( 'NONE',  ( 1.846868145590736310, -27.62500000136559564, 4.458734124999999437 ) ) ;
#9760 = AXIS2_PLACEMENT_3D ( 'NONE', #6331, #11250, #197 ) ;
#9761 = CARTESIAN_POINT ( 'NONE',  ( -2.131511515620587272, -3.916244202832140253, -0.9374999986344056957 ) ) ;
#9762 = ORIENTED_EDGE ( 'NONE', *, *, #2042, .T. ) ;
#9763 = CARTESIAN_POINT ( 'NONE',  ( -7.500000000000001776, 0.000000000000000000, 0.000000000000000000 ) ) ;
#9764 = ORIENTED_EDGE ( 'NONE', *, *, #4218, .F. ) ;
#9765 = ORIENTED_EDGE ( 'NONE', *, *, #10774, .F. ) ;
#9766 = ADVANCED_FACE ( 'NONE', ( #14784 ), #8274, .F. ) ;
#9767 = CARTESIAN_POINT ( 'NONE',  ( 0.000000000000000000, -20.00000000000000000, 0.000000000000000000 ) ) ;
#9768 = AXIS2_PLACEMENT_3D ( 'NONE', #15479, #14414, #4396 ) ;
#9769 = CARTESIAN_POINT ( 'NONE',  ( 4.458734125000000326, -23.37500000136559564, -1.846868145590734978 ) ) ;
#9770 = DIRECTION ( 'NONE',  ( 9.048317650695024227E-15, -0.000000000000000000, 1.000000000000000000 ) ) ;
#9771 = ORIENTED_EDGE ( 'NONE', *, *, #3162, .F. ) ;
#9772 = FACE_OUTER_BOUND ( 'NONE', #2325, .T. ) ;
#9773 = AXIS2_PLACEMENT_3D ( 'NONE', #3163, #13242, #9548 ) ;
#9774 = VECTOR ( 'NONE', #6626, 1000.000000000000000 ) ;
#9775 = PRODUCT ( 'pin2', 'pin2', '', ( #6172 ) ) ;
#9776 = DIRECTION ( 'NONE',  ( -1.000000000000000000, 0.000000000000000000, 0.000000000000000000 ) ) ;
#9777 = FACE_BOUND ( 'NONE', #12736, .T. ) ;
#9778 = SHAPE_REPRESENTATION ( 'Central Drive Wedge _ Scroll Plate', ( #3223 ), #8900 ) ;
#9779 = CARTESIAN_POINT ( 'NONE',  ( -44.43375672972994295, -3.000000000000000000, -22.00000000000000355 ) ) ;
#9780 = CARTESIAN_POINT ( 'NONE',  ( 4.458734124999999437, -21.75000000136559564, 1.846868145590737864 ) ) ;
#9781 = CYLINDRICAL_SURFACE ( 'NONE', #645, 10.00000000000000000 ) ;
#9782 = DIRECTION ( 'NONE',  ( 0.8660254037844387076, 0.000000000000000000, -0.4999999999999997224 ) ) ;
#9783 = CARTESIAN_POINT ( 'NONE',  ( -2.071067811865475061, -29.81250000273118417, -5.000000000000000888 ) ) ;
#9784 = CARTESIAN_POINT ( 'NONE',  ( 2.500000000000000000, 1.178949249685213863, -2.042000000000001148 ) ) ;
#9785 = DIRECTION ( 'NONE',  ( 0.000000000000000000, 0.000000000000000000, 1.000000000000000000 ) ) ;
#9786 = EDGE_CURVE ( 'NONE', #9076, #1108, #1603, .T. ) ;
#9787 = CARTESIAN_POINT ( 'NONE',  ( 3.535533905932738197, -24.87500000000000000, -3.535533905932738197 ) ) ;
#9789 = ADVANCED_FACE ( 'NONE', ( #8815 ), #82, .T. ) ;
#9788 = ORIENTED_EDGE ( 'NONE', *, *, #12740, .T. ) ;
#9790 = EDGE_CURVE ( 'NONE', #1411, #509, #10817, .T. ) ;
#9791 = EDGE_CURVE ( 'NONE', #13808, #10876, #1531, .T. ) ;
#9792 = AXIS2_PLACEMENT_3D ( 'NONE', #7637, #12859, #3008 ) ;
#9793 = FILL_AREA_STYLE ('',( #8749 ) ) ;
#9794 = ORIENTED_EDGE ( 'NONE', *, *, #2450, .F. ) ;
#9795 = LINE ( 'NONE', #4940, #12362 ) ;
#9796 = ORIENTED_EDGE ( 'NONE', *, *, #13213, .T. ) ;
#9797 = CARTESIAN_POINT ( 'NONE',  ( -90.00000000000000000, -34.99999999999999289, -13.35786437626904899 ) ) ;
#9798 = APPLICATION_CONTEXT ( 'automotive_design' ) ;
#9799 = CARTESIAN_POINT ( 'NONE',  ( -2.071067811865450192, -25.43750000273118062, 5.000000000000028422 ) ) ;
#9800 = CARTESIAN_POINT ( 'NONE',  ( 3.033343224707661712, -3.753672977998669946, -2.499999998634408804 ) ) ;
#9801 = DIRECTION ( 'NONE',  ( 0.4999999999999919509, 0.000000000000000000, 0.8660254037844432595 ) ) ;
#9802 = CARTESIAN_POINT ( 'NONE',  ( 2.131511515620586383, 3.916244202832140253, -1.437499998634406140 ) ) ;
#9803 =( NAMED_UNIT ( * ) SI_UNIT ( $, .STERADIAN. ) SOLID_ANGLE_UNIT ( ) );
#9804 = CARTESIAN_POINT ( 'NONE',  ( -39.99999999999999289, -11.00000000000000178, -2.500000000000079492 ) ) ;
#9805 = DIRECTION ( 'NONE',  ( -1.000000000000000000, -0.000000000000000000, -0.000000000000000000 ) ) ;
#9806 = EDGE_CURVE ( 'NONE', #10556, #13119, #244, .T. ) ;
#9807 = ORIENTED_EDGE ( 'NONE', *, *, #15096, .F. ) ;
#9808 = CARTESIAN_POINT ( 'NONE',  ( 4.000000000001088907, 1.658577278524410170, -3.531553309554541720 ) ) ;
#9809 = ORIENTED_EDGE ( 'NONE', *, *, #6093, .T. ) ;
#9810 = ORIENTED_EDGE ( 'NONE', *, *, #14190, .F. ) ;
#9811 = CARTESIAN_POINT ( 'NONE',  ( 3.033343224707661712, -3.753672977998669502, -2.749999998634409248 ) ) ;
#9812 = LINE ( 'NONE', #9503, #13791 ) ;
#9813 = CARTESIAN_POINT ( 'NONE',  ( 3.033343224707661712, -3.753672977998669502, -7.499999998634409692 ) ) ;
#9814 = DIRECTION ( 'NONE',  ( 0.000000000000000000, 1.000000000000000000, 0.000000000000000000 ) ) ;
#9815 = CARTESIAN_POINT ( 'NONE',  ( 2.143131898507869826E-15, 40.00000000000000000, -67.50000000000000000 ) ) ;
#9816 = CARTESIAN_POINT ( 'NONE',  ( 67.49999999999931788, 50.00000000000000000, -2.649999999999964828 ) ) ;
#9817 = CARTESIAN_POINT ( 'NONE',  ( 1.415196051561583790, -4.795541693661363958, -0.1249999972688167760 ) ) ;
#9818 = CARTESIAN_POINT ( 'NONE',  ( -5.000000000000000888, -24.43750000000000355, 2.071067811865474617 ) ) ;
#9819 = PRESENTATION_STYLE_ASSIGNMENT (( #12223 ) ) ;
#9820 = CARTESIAN_POINT ( 'NONE',  ( 3.152801135295367541, -25.56250000136559564, -3.152801135295367541 ) ) ;
#9821 = CARTESIAN_POINT ( 'NONE',  ( -8.190561711645485556E-16, -23.68750000136559564, 4.458734124999999437 ) ) ;
#9822 = CARTESIAN_POINT ( 'NONE',  ( 3.753672977998667726, 3.033343224707664376, -4.249999998634406140 ) ) ;
#9823 = CARTESIAN_POINT ( 'NONE',  ( 30.02221399786053624, -20.00000000000000000, 16.00000000000001421 ) ) ;
#9824 = EDGE_LOOP ( 'NONE', ( #10034, #3310, #4181, #15599 ) ) ;
#9825 = ORIENTED_EDGE ( 'NONE', *, *, #3975, .F. ) ;
#9826 = CARTESIAN_POINT ( 'NONE',  ( 0.000000000000000000, 0.000000000000000000, 0.000000000000000000 ) ) ;
#9827 = ORIENTED_EDGE ( 'NONE', *, *, #5943, .F. ) ;
#9828 = CARTESIAN_POINT ( 'NONE',  ( 3.152801135295367541, -23.56250000136559564, -3.152801135295367541 ) ) ;
#9829 = DIRECTION ( 'NONE',  ( 0.000000000000000000, 0.000000000000000000, 1.000000000000000000 ) ) ;
#9830 = EDGE_CURVE ( 'NONE', #13690, #9986, #7466, .T. ) ;
#9831 = PLANE ( 'NONE',  #8696 ) ;
#9832 = CARTESIAN_POINT ( 'NONE',  ( -120.8578643762690490, -112.8157963042559544, 17.49999999999999289 ) ) ;
#9833 = ADVANCED_FACE ( 'NONE', ( #7601, #6228 ), #12498, .F. ) ;
#9834 = CARTESIAN_POINT ( 'NONE',  ( 5.000000000000000000, -22.06249999999999645, 2.071067811865478614 ) ) ;
#9835 = CARTESIAN_POINT ( 'NONE',  ( 4.209348295687701302, 3.401574460001765665, -1.937500000000002442 ) ) ;
#9836 = DIRECTION ( 'NONE',  ( 0.000000000000000000, 0.000000000000000000, 1.000000000000000000 ) ) ;
#9837 = CARTESIAN_POINT ( 'NONE',  ( -4.257077077555639910, -2.071027201601217893, -0.1914352921446037803 ) ) ;
#9838 = CARTESIAN_POINT ( 'NONE',  ( 1.846868145590736310, -25.62500000136559564, 4.458734124999999437 ) ) ;
#9839 =( BOUNDED_CURVE ( )  B_SPLINE_CURVE ( 3, ( #13239, #5821, #11873, #820 ),
 .UNSPECIFIED., .F., .T. ) 
 B_SPLINE_CURVE_WITH_KNOTS ( ( 4, 4 ),
 ( 0.000000000000000000, 1.570796326794896336 ),
 .UNSPECIFIED. ) 
 CURVE ( )  GEOMETRIC_REPRESENTATION_ITEM ( )  RATIONAL_B_SPLINE_CURVE ( ( 1.000000000000000000, 0.8047378541243650485, 0.8047378541243650485, 1.000000000000000000 ) ) 
 REPRESENTATION_ITEM ( '' )  );
#9840 = CARTESIAN_POINT ( 'NONE',  ( 4.799145180956616130, -0.5093500532425063732, -0.6249999986344092484 ) ) ;
#9841 = ORIENTED_EDGE ( 'NONE', *, *, #14088, .F. ) ;
#9842 = DIRECTION ( 'NONE',  ( 0.000000000000000000, 0.000000000000000000, -1.000000000000000000 ) ) ;
#9843 = ORIENTED_EDGE ( 'NONE', *, *, #1486, .T. ) ;
#9844 = ORIENTED_EDGE ( 'NONE', *, *, #14622, .F. ) ;
#9845 = CARTESIAN_POINT ( 'NONE',  ( -7.922811899608412034, -4.628803996615322269, -8.057669882367653358 ) ) ;
#9846 = CARTESIAN_POINT ( 'NONE',  ( 2.730187237215162345E-16, -23.18750000136559564, -4.458734124999999437 ) ) ;
#9847 = CARTESIAN_POINT ( 'NONE',  ( -31.74999999999995737, 0.000000000000000000, 0.000000000000000000 ) ) ;
#9848 = EDGE_LOOP ( 'NONE', ( #11824, #5051, #3887, #7801, #11843 ) ) ;
#9849 = DIRECTION ( 'NONE',  ( 0.8660254037844385966, 0.000000000000000000, 0.5000000000000003331 ) ) ;
#9850 = VECTOR ( 'NONE', #517, 1000.000000000000000 ) ;
#9851 = CARTESIAN_POINT ( 'NONE',  ( 0.000000000000000000, -20.00000000000000000, 0.000000000000000000 ) ) ;
#9852 = EDGE_CURVE ( 'NONE', #9569, #865, #9273, .T. ) ;
#9853 = DIRECTION ( 'NONE',  ( 0.000000000000000000, 0.000000000000000000, -1.000000000000000000 ) ) ;
#9854 = DIRECTION ( 'NONE',  ( 0.8191520442889907994, 0.000000000000000000, 0.5735764363510474917 ) ) ;
#9855 = EDGE_CURVE ( 'NONE', #12513, #5598, #12663, .T. ) ;
#9856 = CARTESIAN_POINT ( 'NONE',  ( 4.458734125000000326, -24.62500000136559564, -1.846868145590734978 ) ) ;
#9857 = DIRECTION ( 'NONE',  ( 0.000000000000000000, 0.000000000000000000, 1.000000000000000000 ) ) ;
#9858 = CARTESIAN_POINT ( 'NONE',  ( -19.99999999999956657, -13.00000000000000178, 8.786575603324269439E-13 ) ) ;
#9859 = CARTESIAN_POINT ( 'NONE',  ( 5.000000000000000000, -29.18750000273119127, 2.071067811865478614 ) ) ;
#9860 = LINE ( 'NONE', #13649, #2914 ) ;
#9861 = CARTESIAN_POINT ( 'NONE',  ( 3.535533905932736864, -24.25000000273118772, 3.535533905932738641 ) ) ;
#9862 = SURFACE_SIDE_STYLE ('',( #2660 ) ) ;
#9863 = ORIENTED_EDGE ( 'NONE', *, *, #1259, .F. ) ;
#9864 = ORIENTED_EDGE ( 'NONE', *, *, #1732, .F. ) ;
#9865 = LINE ( 'NONE', #11088, #522 ) ;
#9866 = EDGE_LOOP ( 'NONE', ( #6615, #14968, #7592, #1024 ) ) ;
#9867 = DIRECTION ( 'NONE',  ( 0.000000000000000000, 1.000000000000000000, 0.000000000000000000 ) ) ;
#9868 = B_SPLINE_CURVE_WITH_KNOTS ( 'NONE', 3,
 ( #11528, #3054, #7998, #7764, #9287, #7836 ),
 .UNSPECIFIED., .F., .F.,
 ( 4, 2, 4 ),
 ( -5.145455527303427788E-06, 0.0004153350442917243344, 0.0008358155441107501145 ),
 .UNSPECIFIED. ) ;
#9869 = EDGE_CURVE ( 'NONE', #9381, #11190, #7803, .T. ) ;
#9870 = ADVANCED_FACE ( 'NONE', ( #15104 ), #9928, .F. ) ;
#9871 = CARTESIAN_POINT ( 'NONE',  ( 0.2500000000000002220, 5.204748896376250699E-16, -4.250000000000000000 ) ) ;
#9872 = CIRCLE ( 'NONE', #7299, 0.2500000000000002220 ) ;
#9873 = CIRCLE ( 'NONE', #13215, 2.649999999999985700 ) ;
#9874 = CARTESIAN_POINT ( 'NONE',  ( -0.5093500532425060401, -4.799145180956616130, -2.624999998634407028 ) ) ;
#9875 = APPLICATION_PROTOCOL_DEFINITION ( 'draft international standard', 'automotive_design', 1998, #8064 ) ;
#9876 = CARTESIAN_POINT ( 'NONE',  ( -3.753672977998669946, -3.033343224707661712, -5.999999998634407916 ) ) ;
#9877 = LINE ( 'NONE', #13579, #5906 ) ;
#9878 = DIRECTION ( 'NONE',  ( -0.000000000000000000, 1.000000000000000000, -0.000000000000000000 ) ) ;
#9879 = VECTOR ( 'NONE', #3616, 999.9999999999998863 ) ;
#9880 = ORIENTED_EDGE ( 'NONE', *, *, #8040, .T. ) ;
#9881 = CARTESIAN_POINT ( 'NONE',  ( 2.500000000000000000, -1.178949249685213863, 2.042000000000002924 ) ) ;
#9882 = ORIENTED_EDGE ( 'NONE', *, *, #3082, .F. ) ;
#9883 = ORIENTED_EDGE ( 'NONE', *, *, #8811, .T. ) ;
#9884 = CARTESIAN_POINT ( 'NONE',  ( 4.276409079477644148, 1.261996585732577891, -4.562499998634405252 ) ) ;
#9885 = CARTESIAN_POINT ( 'NONE',  ( 4.000000000000000000, 2.309401076758515803, -0.4999999999999995559 ) ) ;
#9886 = EDGE_CURVE ( 'NONE', #2474, #2543, #6955, .T. ) ;
#9887 = FACE_OUTER_BOUND ( 'NONE', #14446, .T. ) ;
#9888 = CARTESIAN_POINT ( 'NONE',  ( 0.000000000000000000, -11.00000000000000178, 0.000000000000000000 ) ) ;
#9889 = CARTESIAN_POINT ( 'NONE',  ( -6.765421556309547668E-13, 37.00000000000000000, 64.84999999999931219 ) ) ;
#9890 = CARTESIAN_POINT ( 'NONE',  ( -2.071067811865469288, -30.43750000273118772, 5.000000000000007994 ) ) ;
#9891 = CARTESIAN_POINT ( 'NONE',  ( -2.390265326283148806, -4.391654775818394363, -0.2499999972688168870 ) ) ;
#9892 = PLANE ( 'NONE',  #4870 ) ;
#9893 = CYLINDRICAL_SURFACE ( 'NONE', #2272, 40.00000000000000711 ) ;
#9894 = CARTESIAN_POINT ( 'NONE',  ( 1.846868145590736310, -26.87500000136559919, 4.458734124999997661 ) ) ;
#9895 = CARTESIAN_POINT ( 'NONE',  ( 3.152801135295366208, -22.56250000136559564, 3.152801135295367985 ) ) ;
#9896 = CARTESIAN_POINT ( 'NONE',  ( -2.131511515620587272, -3.916244202832140253, -2.687499998634407028 ) ) ;
#9897 = LINE ( 'NONE', #14836, #5831 ) ;
#9898 = ORIENTED_EDGE ( 'NONE', *, *, #846, .F. ) ;
#9899 = EDGE_LOOP ( 'NONE', ( #11472, #4900, #11379, #659, #10076, #12380, #13566 ) ) ;
#9900 = SURFACE_SIDE_STYLE ('',( #13610 ) ) ;
#9901 = ORIENTED_EDGE ( 'NONE', *, *, #656, .F. ) ;
#9902 = CARTESIAN_POINT ( 'NONE',  ( 3.535533905932738197, -31.00000000273118772, -3.535533905932738197 ) ) ;
#9903 = FACE_OUTER_BOUND ( 'NONE', #6897, .T. ) ;
#9904 = DIRECTION ( 'NONE',  ( 0.000000000000000000, 0.000000000000000000, 1.000000000000000000 ) ) ;
#9905 = ADVANCED_FACE ( 'NONE', ( #7772 ), #7522, .T. ) ;
#9906 = DIRECTION ( 'NONE',  ( -1.000000000000000000, -0.000000000000000000, -0.000000000000000000 ) ) ;
#9907 = DIRECTION ( 'NONE',  ( -1.000000000000000000, -1.734723475976808080E-15, 0.000000000000000000 ) ) ;
#9908 = CIRCLE ( 'NONE', #3717, 9.999999999999980460 ) ;
#9909 = CARTESIAN_POINT ( 'NONE',  ( -116.3391301858327296, -120.2076149402627294, 7.500000000000001776 ) ) ;
#9910 = CARTESIAN_POINT ( 'NONE',  ( -1.415196051561583790, 4.795541693661363958, 0.2499999999999967526 ) ) ;
#9911 = CARTESIAN_POINT ( 'NONE',  ( 2.500000000000000000, -2.357898499370432610, 3.252606517456513302E-15 ) ) ;
#9912 = CARTESIAN_POINT ( 'NONE',  ( -3.472371940586054251, -2.614027278893156669, -3.320322319202162031 ) ) ;
#9913 = CARTESIAN_POINT ( 'NONE',  ( 3.152801135295367541, -27.31250000136559564, -3.152801135295367541 ) ) ;
#9914 = CARTESIAN_POINT ( 'NONE',  ( -3.753672977998669946, -3.033343224707661712, -0.9999999986344076941 ) ) ;
#9915 = ORIENTED_EDGE ( 'NONE', *, *, #3634, .T. ) ;
#9916 = DIRECTION ( 'NONE',  ( 0.000000000000000000, 0.000000000000000000, -1.000000000000000000 ) ) ;
#9917 = ORIENTED_EDGE ( 'NONE', *, *, #12980, .F. ) ;
#9918 = ORIENTED_EDGE ( 'NONE', *, *, #12068, .T. ) ;
#9919 = CARTESIAN_POINT ( 'NONE',  ( -4.203934362469166963, -1.640673743454851286, -3.598432614606932756 ) ) ;
#9920 = B_SPLINE_CURVE_WITH_KNOTS ( 'NONE', 3,
 ( #15338, #1901, #6847, #11912, #11754, #12890 ),
 .UNSPECIFIED., .F., .F.,
 ( 4, 2, 4 ),
 ( 2.475503369187537856E-07, 0.002222330217055623267, 0.004444412883774327173 ),
 .UNSPECIFIED. ) ;
#9921 = AXIS2_PLACEMENT_3D ( 'NONE', #3410, #4787, #13180 ) ;
#9922 = CARTESIAN_POINT ( 'NONE',  ( 4.458734125000000326, -24.37500000136559564, -1.846868145590734978 ) ) ;
#9923 = ADVANCED_FACE ( 'NONE', ( #11459 ), #3873, .T. ) ;
#9924 = FACE_OUTER_BOUND ( 'NONE', #9342, .T. ) ;
#9925 = AXIS2_PLACEMENT_3D ( 'NONE', #10883, #15824, #2385 ) ;
#9926 = ORIENTED_EDGE ( 'NONE', *, *, #2927, .F. ) ;
#9927 = CARTESIAN_POINT ( 'NONE',  ( 5.000000000000004441, -2.247904837838113790E-16, -6.920263044861760804 ) ) ;
#9928 = PLANE ( 'NONE',  #6429 ) ;
#9929 = FACE_BOUND ( 'NONE', #1910, .T. ) ;
#9930 = DIRECTION ( 'NONE',  ( 0.000000000000000000, 1.000000000000000000, 0.000000000000000000 ) ) ;
#9931 =( BOUNDED_CURVE ( )  B_SPLINE_CURVE ( 2, ( #4166, #4339, #1821, #2949, #11672, #627, #10481, #9347, #15414 ),
 .UNSPECIFIED., .F., .F. ) 
 B_SPLINE_CURVE_WITH_KNOTS ( ( 3, 2, 2, 2, 3 ),
 ( 0.4750000000000000888, 0.4875000000000000999, 0.5000000000000001110, 0.5125000000000000666, 0.5250000000000001332 ),
 .UNSPECIFIED. ) 
 CURVE ( )  GEOMETRIC_REPRESENTATION_ITEM ( )  RATIONAL_B_SPLINE_CURVE ( ( 0.9999999999999993339, 0.9238795325112874046, 1.000000000000000000, 0.9238795325112867385, 1.000000000000000000, 0.9238795325112867385, 1.000000000000000000, 0.9238795325112860723, 1.000000000000000666 ) ) 
 REPRESENTATION_ITEM ( '' )  );
#9932 = CARTESIAN_POINT ( 'NONE',  ( 5.000000000000000888, -28.93750000000000355, -2.071067811865475505 ) ) ;
#9933 = CIRCLE ( 'NONE', #142, 2.500000000000909495 ) ;
#9934 = DIRECTION ( 'NONE',  ( 0.000000000000000000, -0.000000000000000000, 1.000000000000000000 ) ) ;
#9935 = CARTESIAN_POINT ( 'NONE',  ( 4.000000000000000000, 2.309401076758497151, -3.433295621305379353 ) ) ;
#9936 = CARTESIAN_POINT ( 'NONE',  ( 3.061616997868383141E-16, -26.87500000273118772, -5.000000000000000000 ) ) ;
#9937 =( GEOMETRIC_REPRESENTATION_CONTEXT ( 3 ) GLOBAL_UNCERTAINTY_ASSIGNED_CONTEXT ( ( #5639 ) ) GLOBAL_UNIT_ASSIGNED_CONTEXT ( ( #2925, #4145, #4310 ) ) REPRESENTATION_CONTEXT ( 'NONE', 'WORKASPACE' ) );
#9938 = CARTESIAN_POINT ( 'NONE',  ( 6.123233995736766282E-16, -20.00000000000000000, -5.000000000000000000 ) ) ;
#9939 = CARTESIAN_POINT ( 'NONE',  ( -4.458734124999999437, -31.00000000136559564, -1.846868145590735644 ) ) ;
#9940 = DIRECTION ( 'NONE',  ( 0.000000000000000000, 0.000000000000000000, -1.000000000000000000 ) ) ;
#9941 = ORIENTED_EDGE ( 'NONE', *, *, #5179, .T. ) ;
#9943 = ORIENTED_EDGE ( 'NONE', *, *, #11652, .T. ) ;
#9942 = ADVANCED_FACE ( 'NONE', ( #12425 ), #7923, .F. ) ;
#9944 = CARTESIAN_POINT ( 'NONE',  ( 0.2500000000000002220, 0.000000000000000000, 4.250000000000000000 ) ) ;
#9945 = EDGE_CURVE ( 'NONE', #11703, #1559, #10347, .T. ) ;
#9946 = CIRCLE ( 'NONE', #3743, 2.041999999999999815 ) ;
#9947 = ORIENTED_EDGE ( 'NONE', *, *, #5905, .T. ) ;
#9948 = LINE ( 'NONE', #3356, #3516 ) ;
#9949 = AXIS2_PLACEMENT_3D ( 'NONE', #4845, #1197, #4681 ) ;
#9950 = VECTOR ( 'NONE', #4998, 1000.000000000000000 ) ;
#9951 = CARTESIAN_POINT ( 'NONE',  ( 39.90939079054413696, -3.661800705854930893, 28.10922023582534379 ) ) ;
#9952 = CARTESIAN_POINT ( 'NONE',  ( -1.261996585732579224, 4.276409079477648589, -4.062499998634405252 ) ) ;
#9953 = DIRECTION ( 'NONE',  ( 6.982962677686266711E-15, 0.000000000000000000, -1.000000000000000000 ) ) ;
#9954 = VECTOR ( 'NONE', #6297, 1000.000000000000114 ) ;
#9955 = CARTESIAN_POINT ( 'NONE',  ( -4.799145180956616130, 0.5093500532425063732, -4.124999998634405252 ) ) ;
#9956 = PLANE ( 'NONE',  #4812 ) ;
#9957 = CARTESIAN_POINT ( 'NONE',  ( 5.000000000000000888, -23.93750000000000355, -2.071067811865475505 ) ) ;
#9958 = EDGE_LOOP ( 'NONE', ( #11471, #12098, #13111, #578 ) ) ;
#9959 = VECTOR ( 'NONE', #1336, 1000.000000000000000 ) ;
#9960 = CARTESIAN_POINT ( 'NONE',  ( 67.49999999999931788, 40.00000000000000000, 2.650000000000013678 ) ) ;
#9961 = EDGE_CURVE ( 'NONE', #15162, #5750, #12603, .T. ) ;
#9962 = ORIENTED_EDGE ( 'NONE', *, *, #12479, .F. ) ;
#9963 = DIRECTION ( 'NONE',  ( -1.000000000000000000, 0.000000000000000000, -3.343241100358131282E-16 ) ) ;
#9964 = DIRECTION ( 'NONE',  ( -1.000000000000000000, -0.000000000000000000, -0.000000000000000000 ) ) ;
#9965 = EDGE_CURVE ( 'NONE', #1559, #4540, #7925, .T. ) ;
#9966 = ORIENTED_EDGE ( 'NONE', *, *, #2659, .F. ) ;
#9967 = CONTEXT_DEPENDENT_SHAPE_REPRESENTATION ( #8285, #10247 ) ;
#9968 = CARTESIAN_POINT ( 'NONE',  ( -1.261996585732579224, 4.276409079477648589, -2.312499998634407028 ) ) ;
#9969 = CARTESIAN_POINT ( 'NONE',  ( 4.000000000000000000, 0.9868501483902631932, -0.09357334158579604100 ) ) ;
#9970 = PRODUCT_DEFINITION_SHAPE ( 'NONE', 'NONE',  #15990 ) ;
#9971 = VECTOR ( 'NONE', #15081, 1000.000000000000000 ) ;
#9972 = CYLINDRICAL_SURFACE ( 'NONE', #12084, 2.649999999999992806 ) ;
#9973 = DIRECTION ( 'NONE',  ( -0.8660254037844385966, -0.5000000000000001110, 0.000000000000000000 ) ) ;
#9974 = PRODUCT_DEFINITION_CONTEXT ( 'detailed design', #14975, 'design' ) ;
#9975 = DIRECTION ( 'NONE',  ( -1.000000000000000000, -0.000000000000000000, -0.000000000000000000 ) ) ;
#9976 = CARTESIAN_POINT ( 'NONE',  ( -3.401574460001764777, 4.209348295687701302, -4.562499997268816720 ) ) ;
#9977 = FACE_OUTER_BOUND ( 'NONE', #13204, .T. ) ;
#9978 = AXIS2_PLACEMENT_3D ( 'NONE', #8066, #11751, #10573 ) ;
#9979 = CARTESIAN_POINT ( 'NONE',  ( 5.000000000000000000, -28.12500000273118772, 0.000000000000000000 ) ) ;
#9980 = CARTESIAN_POINT ( 'NONE',  ( 4.458734124999997661, -27.75000000136559564, 1.846868145590737864 ) ) ;
#9981 = VERTEX_POINT ( 'NONE', #9296 ) ;
#9982 = DIRECTION ( 'NONE',  ( 0.000000000000000000, 1.000000000000000000, 0.000000000000000000 ) ) ;
#9983 = CARTESIAN_POINT ( 'NONE',  ( 3.916244202832140253, -2.131511515620588160, -4.437499998634405252 ) ) ;
#9984 = LINE ( 'NONE', #1330, #15131 ) ;
#9985 = EDGE_CURVE ( 'NONE', #6711, #3387, #8084, .T. ) ;
#9986 = VERTEX_POINT ( 'NONE', #13064 ) ;
#9987 = ORIENTED_EDGE ( 'NONE', *, *, #9269, .T. ) ;
#9988 = EDGE_CURVE ( 'NONE', #10876, #13011, #2035, .T. ) ;
#9989 = PRODUCT_DEFINITION_FORMATION_WITH_SPECIFIED_SOURCE ( 'ANY', '', #2282, .NOT_KNOWN. ) ;
#9990 = CIRCLE ( 'NONE', #12040, 5.000000000000000000 ) ;
#9991 = EDGE_CURVE ( 'NONE', #13263, #6791, #15470, .T. ) ;
#9992 = SURFACE_STYLE_USAGE ( .BOTH. , #9900 ) ;
#9993 = ORIENTED_EDGE ( 'NONE', *, *, #11179, .T. ) ;
#9994 = AXIS2_PLACEMENT_3D ( 'NONE', #287, #1479, #5275 ) ;
#9995 = CARTESIAN_POINT ( 'NONE',  ( 4.458734124999999437, -23.75000000136559208, 1.846868145590737864 ) ) ;
#9996 = CARTESIAN_POINT ( 'NONE',  ( 2.500000000000000000, -2.357898499370432610, 3.252606517456513302E-15 ) ) ;
#9997 = FACE_OUTER_BOUND ( 'NONE', #1412, .T. ) ;
#9998 = CARTESIAN_POINT ( 'NONE',  ( -35.00000000000000000, 50.00000000000000000, 0.000000000000000000 ) ) ;
#9999 = CARTESIAN_POINT ( 'NONE',  ( 19.99999999999956657, -8.786575603324269439E-13, -4.500000000000000000 ) ) ;
#10000 = DIRECTION ( 'NONE',  ( 0.000000000000000000, 0.000000000000000000, 1.000000000000000000 ) ) ;
#10001 = CARTESIAN_POINT ( 'NONE',  ( -3.401574460001764777, 4.209348295687701302, -5.687500000000003553 ) ) ;
#10002 = CARTESIAN_POINT ( 'NONE',  ( -91.33974596215560382, -110.0591436588189396, -7.500000000000000000 ) ) ;
#10003 = CARTESIAN_POINT ( 'NONE',  ( 3.152801135295366208, -25.56250000136559564, 3.152801135295367985 ) ) ;
#10004 = CARTESIAN_POINT ( 'NONE',  ( -3.916244202832140253, 2.131511515620587272, -3.187499998634407916 ) ) ;
#10005 = ORIENTED_EDGE ( 'NONE', *, *, #15096, .T. ) ;
#10006 = AXIS2_PLACEMENT_3D ( 'NONE', #4030, #6312, #8821 ) ;
#10007 = CARTESIAN_POINT ( 'NONE',  ( 35.00000000000000000, 37.00000000000000000, -5.999999999999991118 ) ) ;
#10008 = VERTEX_POINT ( 'NONE', #1917 ) ;
#10009 = ORIENTED_EDGE ( 'NONE', *, *, #12929, .T. ) ;
#10010 = DIRECTION ( 'NONE',  ( -0.8660254037844383745, -0.000000000000000000, -0.5000000000000005551 ) ) ;
#10011 = VECTOR ( 'NONE', #11567, 1000.000000000000000 ) ;
#10012 = B_SPLINE_CURVE_WITH_KNOTS ( 'NONE', 3,
 ( #10538, #15385, #7056, #3337, #9555, #10688, #11883, #11804 ),
 .UNSPECIFIED., .F., .F.,
 ( 4, 2, 2, 4 ),
 ( 0.005725059856848641743, 0.006314084072593626612, 0.006903108288338611481, 0.008081156719828581220 ),
 .UNSPECIFIED. ) ;
#10013 = EDGE_CURVE ( 'NONE', #12457, #5598, #4432, .T. ) ;
#10014 = CARTESIAN_POINT ( 'NONE',  ( -3.152801135295367985, -24.81250000136559564, 3.152801135295367096 ) ) ;
#10015 = CARTESIAN_POINT ( 'NONE',  ( -19.99999999999956657, -13.00000000000000178, 2.500000000000877520 ) ) ;
#10016 = ORIENTED_EDGE ( 'NONE', *, *, #15078, .F. ) ;
#10017 = AXIS2_PLACEMENT_3D ( 'NONE', #9471, #5989, #11880 ) ;
#10018 = DIRECTION ( 'NONE',  ( 0.000000000000000000, 0.000000000000000000, 1.000000000000000000 ) ) ;
#10019 = EDGE_CURVE ( 'NONE', #717, #11587, #11323, .T. ) ;
#10021 = AXIS2_PLACEMENT_3D ( 'NONE', #7087, #1017, #13433 ) ;
#10020 = DIRECTION ( 'NONE',  ( -1.000000000000000000, 0.000000000000000000, -1.114413700119375779E-16 ) ) ;
#10022 = CARTESIAN_POINT ( 'NONE',  ( -4.276409079477644148, -1.261996585732578335, -2.812499998634407472 ) ) ;
#10023 = CARTESIAN_POINT ( 'NONE',  ( 4.339338055002142092, 1.058955340485046692, -0.3789984458506918119 ) ) ;
#10024 = CIRCLE ( 'NONE', #15164, 75.00000000000001421 ) ;
#10025 = CARTESIAN_POINT ( 'NONE',  ( -5.000000000000000000, -30.50000000000000000, -6.123233995736766282E-16 ) ) ;
#10026 = CARTESIAN_POINT ( 'NONE',  ( 17.99999999999957012, -8.784126309725975241E-13, -11.50000000000000000 ) ) ;
#10027 = ADVANCED_FACE ( 'NONE', ( #567 ), #2002, .F. ) ;
#10028 = CARTESIAN_POINT ( 'NONE',  ( -91.33974596215558961, -105.7735026918962546, -7.500000000000000000 ) ) ;
#10029 = CARTESIAN_POINT ( 'NONE',  ( 3.061616997868383141E-16, -29.87500000273118417, -5.000000000000000000 ) ) ;
#10030 = DIRECTION ( 'NONE',  ( -0.000000000000000000, 1.000000000000000000, -0.000000000000000000 ) ) ;
#10031 = VECTOR ( 'NONE', #13185, 1000.000000000000000 ) ;
#10032 = CARTESIAN_POINT ( 'NONE',  ( 1.846868145590735200, -30.25000000136559919, -4.458734124999999437 ) ) ;
#10033 = CARTESIAN_POINT ( 'NONE',  ( 67.49999999999931788, 50.00000000000000000, -2.649999999999971934 ) ) ;
#10034 = ORIENTED_EDGE ( 'NONE', *, *, #15783, .F. ) ;
#10035 = ORIENTED_EDGE ( 'NONE', *, *, #2834, .F. ) ;
#10036 = VERTEX_POINT ( 'NONE', #3064 ) ;
#10037 = CARTESIAN_POINT ( 'NONE',  ( -41.99999999999978684, -11.00000000000000178, 3.499999999999998668 ) ) ;
#10038 = VECTOR ( 'NONE', #936, 1000.000000000000000 ) ;
#10039 = CIRCLE ( 'NONE', #11831, 5.000000000000000000 ) ;
#10040 = ORIENTED_EDGE ( 'NONE', *, *, #7227, .F. ) ;
#10041 = FACE_OUTER_BOUND ( 'NONE', #10173, .T. ) ;
#10042 = VECTOR ( 'NONE', #6488, 1000.000000000000000 ) ;
#10043 = EDGE_CURVE ( 'NONE', #1654, #9678, #15214, .T. ) ;
#10044 = CARTESIAN_POINT ( 'NONE',  ( -4.458734125000001214, -31.12500000136559564, 1.846868145590734089 ) ) ;
#10045 = ADVANCED_FACE ( 'NONE', ( #6951 ), #11852, .T. ) ;
#10046 = AXIS2_PLACEMENT_3D ( 'NONE', #14790, #11081, #14634 ) ;
#10047 = EDGE_CURVE ( 'NONE', #7770, #6730, #7039, .T. ) ;
#10048 = CARTESIAN_POINT ( 'NONE',  ( 4.276409079477644148, 1.261996585732577891, -6.562499998634407028 ) ) ;
#10049 = CARTESIAN_POINT ( 'NONE',  ( -28.86751345948129455, -20.00000000000000000, 49.99999999999999289 ) ) ;
#10050 = FACE_OUTER_BOUND ( 'NONE', #12900, .T. ) ;
#10051 = ORIENTED_EDGE ( 'NONE', *, *, #9169, .T. ) ;
#10052 = LINE ( 'NONE', #14983, #235 ) ;
#10053 =( LENGTH_UNIT ( ) NAMED_UNIT ( * ) SI_UNIT ( .MILLI., .METRE. ) );
#10054 = EDGE_LOOP ( 'NONE', ( #7174, #10132, #15157, #2662 ) ) ;
#10055 = DIRECTION ( 'NONE',  ( 0.000000000000000000, -0.4999999999999992784, 0.8660254037844389297 ) ) ;
#10056 = LINE ( 'NONE', #10131, #1191 ) ;
#10057 = ORIENTED_EDGE ( 'NONE', *, *, #4479, .F. ) ;
#10058 = CONTEXT_DEPENDENT_SHAPE_REPRESENTATION ( #832, #12406 ) ;
#10059 = CARTESIAN_POINT ( 'NONE',  ( -4.276409079477644148, -1.261996585732578335, -6.062499998634407028 ) ) ;
#10060 = CARTESIAN_POINT ( 'NONE',  ( 2.500000000000000000, 2.357898499370433054, -1.951563910473907981E-15 ) ) ;
#10061 = TOROIDAL_SURFACE ( 'NONE', #15224, 10.12668159690567649, 0.7733184030943209830 ) ;
#10062 = CARTESIAN_POINT ( 'NONE',  ( -5.000000000000000888, 6.123233995736767268E-16, -25.03750572909317285 ) ) ;
#10063 = DIRECTION ( 'NONE',  ( -0.8660254037844385966, 0.000000000000000000, -0.5000000000000002220 ) ) ;
#10064 = EDGE_CURVE ( 'NONE', #8029, #10306, #2872, .T. ) ;
#10065 = PRODUCT_RELATED_PRODUCT_CATEGORY ( 'part', '', ( #9775 ) ) ;
#10066 = CARTESIAN_POINT ( 'NONE',  ( 2.500000000000000000, 1.768423874527824902, 1.020999999999999019 ) ) ;
#10067 = CARTESIAN_POINT ( 'NONE',  ( -4.391654775818395251, 2.390265326283148806, -4.499999997268817609 ) ) ;
#10068 = DIRECTION ( 'NONE',  ( 0.000000000000000000, 0.000000000000000000, -1.000000000000000000 ) ) ;
#10069 = CARTESIAN_POINT ( 'NONE',  ( -2.104132545462253034, 4.020150199444661787, -0.3258662981471979747 ) ) ;
#10070 = CARTESIAN_POINT ( 'NONE',  ( 4.769696007084728073, -20.00000000000000000, -1.500000000000000000 ) ) ;
#10071 = ORIENTED_EDGE ( 'NONE', *, *, #5295, .T. ) ;
#10072 = DIRECTION ( 'NONE',  ( 0.000000000000000000, 0.000000000000000000, -1.000000000000000000 ) ) ;
#10073 = CARTESIAN_POINT ( 'NONE',  ( -4.197393957002303999, 0.4069871074557429025, -3.503767560748926257 ) ) ;
#10074 = VECTOR ( 'NONE', #5688, 1000.000000000000000 ) ;
#10075 = CARTESIAN_POINT ( 'NONE',  ( -4.000000000000004441, 2.309401076758496263, -3.504269196027523847 ) ) ;
#10076 = ORIENTED_EDGE ( 'NONE', *, *, #12141, .T. ) ;
#10077 = EDGE_LOOP ( 'NONE', ( #26, #6556, #14624 ) ) ;
#10078 =( NAMED_UNIT ( * ) PLANE_ANGLE_UNIT ( ) SI_UNIT ( $, .RADIAN. ) );
#10079 = ORIENTED_EDGE ( 'NONE', *, *, #145, .F. ) ;
#10080 = DIRECTION ( 'NONE',  ( 1.000000000000000000, 0.000000000000000000, 0.000000000000000000 ) ) ;
#10081 = CARTESIAN_POINT ( 'NONE',  ( 0.000000000000000000, -13.00000000000000178, 0.000000000000000000 ) ) ;
#10082 = DIRECTION ( 'NONE',  ( 0.000000000000000000, -1.000000000000000000, 1.287488025362403787E-15 ) ) ;
#10083 = EDGE_CURVE ( 'NONE', #10415, #8643, #9382, .T. ) ;
#10084 = CARTESIAN_POINT ( 'NONE',  ( 3.535533905932738197, -25.87500000000000355, -3.535533905932738197 ) ) ;
#10085 = CARTESIAN_POINT ( 'NONE',  ( -1.060314165522904917, -8.048081368953686976, -7.659344964963222147 ) ) ;
#10086 = EDGE_CURVE ( 'NONE', #3779, #7837, #740, .T. ) ;
#10087 = FACE_OUTER_BOUND ( 'NONE', #526, .T. ) ;
#10088 = CARTESIAN_POINT ( 'NONE',  ( -1.415196051561583790, 4.795541693661363958, -6.750000000000002665 ) ) ;
#10089 = CARTESIAN_POINT ( 'NONE',  ( 5.000000000000000888, -29.93750000000000355, -2.071067811865475505 ) ) ;
#10090 = CARTESIAN_POINT ( 'NONE',  ( -0.5449313310646672903, -4.304185902836978883, -3.316620875263469159 ) ) ;
#10091 = CARTESIAN_POINT ( 'NONE',  ( -3.152801135295367096, -25.06250000136559564, -3.152801135295367541 ) ) ;
#10092 = CARTESIAN_POINT ( 'NONE',  ( -3.916244202832140253, 2.131511515620587272, -7.187499998634407916 ) ) ;
#10093 = VERTEX_POINT ( 'NONE', #661 ) ;
#10094 = FACE_OUTER_BOUND ( 'NONE', #10096, .T. ) ;
#10095 = VERTEX_POINT ( 'NONE', #15604 ) ;
#10096 = EDGE_LOOP ( 'NONE', ( #3970, #15916, #7679, #15190, #3479, #9495, #11946 ) ) ;
#10097 = CARTESIAN_POINT ( 'NONE',  ( 4.458734124999999437, -21.43750000136559208, 0.000000000000000000 ) ) ;
#10098 = ORIENTED_EDGE ( 'NONE', *, *, #2772, .F. ) ;
#10099 = DIRECTION ( 'NONE',  ( -0.000000000000000000, -1.000000000000000000, -0.000000000000000000 ) ) ;
#10100 = CARTESIAN_POINT ( 'NONE',  ( -8.673617379884035472E-16, -9.147862274876560562, -8.047472243342939535 ) ) ;
#10101 = CARTESIAN_POINT ( 'NONE',  ( 1.261996585732578113, -4.276409079477644148, -1.562499998634406140 ) ) ;
#10102 = DIRECTION ( 'NONE',  ( 1.000000000000000000, 0.000000000000000000, 0.000000000000000000 ) ) ;
#10103 = EDGE_CURVE ( 'NONE', #14425, #6438, #6882, .T. ) ;
#10104 = CARTESIAN_POINT ( 'NONE',  ( 2.071067811865475505, -28.81250000000000355, -5.000000000000000888 ) ) ;
#10105 = CARTESIAN_POINT ( 'NONE',  ( -3.750000000000000000, -6.495190528383298023, -6.991905250253757309 ) ) ;
#10106 = CARTESIAN_POINT ( 'NONE',  ( 35.00000000000000000, 37.00000000000000000, 5.999999999999991118 ) ) ;
#10107 = CARTESIAN_POINT ( 'NONE',  ( 5.000000000000000000, -27.18750000273119127, 2.071067811865478614 ) ) ;
#10108 = CARTESIAN_POINT ( 'NONE',  ( 0.2500000000000002220, 0.000000000000000000, 4.000000000000000000 ) ) ;
#10109 = CARTESIAN_POINT ( 'NONE',  ( 5.000000000000000888, -24.06250000273118772, -2.071067811865475505 ) ) ;
#10110 = DIRECTION ( 'NONE',  ( 1.000000000000000000, 0.000000000000000000, 0.000000000000000000 ) ) ;
#10111 = B_SPLINE_CURVE_WITH_KNOTS ( 'NONE', 3,
 ( #9716, #7150, #7071, #7304, #8448, #11892 ),
 .UNSPECIFIED., .F., .F.,
 ( 4, 2, 4 ),
 ( 0.004444412883774327173, 0.006655097293744434601, 0.008865781703714541162 ),
 .UNSPECIFIED. ) ;
#10112 = ORIENTED_EDGE ( 'NONE', *, *, #9740, .T. ) ;
#10113 = VERTEX_POINT ( 'NONE', #15529 ) ;
#10114 =( LENGTH_UNIT ( ) NAMED_UNIT ( * ) SI_UNIT ( .MILLI., .METRE. ) );
#10115 = ORIENTED_EDGE ( 'NONE', *, *, #4381, .T. ) ;
#10116 = DIRECTION ( 'NONE',  ( -0.4999999999999997224, 0.000000000000000000, -0.8660254037844388186 ) ) ;
#10117 = ORIENTED_EDGE ( 'NONE', *, *, #12499, .F. ) ;
#10118 = DIRECTION ( 'NONE',  ( -0.000000000000000000, -1.000000000000000000, -0.000000000000000000 ) ) ;
#10119 = DIRECTION ( 'NONE',  ( -0.000000000000000000, -0.000000000000000000, 1.000000000000000000 ) ) ;
#10120 = DIRECTION ( 'NONE',  ( 0.000000000000000000, 1.000000000000000000, 0.000000000000000000 ) ) ;
#10121 = VECTOR ( 'NONE', #3469, 1000.000000000000000 ) ;
#10122 = CARTESIAN_POINT ( 'NONE',  ( -35.00000000000000000, 32.00000000000000000, 6.938893903907228378E-15 ) ) ;
#10123 = CARTESIAN_POINT ( 'NONE',  ( -1.261996585732579224, 4.276409079477648589, -7.312499998634407916 ) ) ;
#10124 = FACE_OUTER_BOUND ( 'NONE', #6774, .T. ) ;
#10125 = LINE ( 'NONE', #14734, #14665 ) ;
#10126 = VERTEX_POINT ( 'NONE', #1853 ) ;
#10127 = FACE_OUTER_BOUND ( 'NONE', #10668, .T. ) ;
#10128 =( NAMED_UNIT ( * ) PLANE_ANGLE_UNIT ( ) SI_UNIT ( $, .RADIAN. ) );
#10129 = VERTEX_POINT ( 'NONE', #4523 ) ;
#10130 = FACE_OUTER_BOUND ( 'NONE', #9086, .T. ) ;
#10131 = CARTESIAN_POINT ( 'NONE',  ( 12.67949192431120764, -5.000000000000000000, 61.96152422706632024 ) ) ;
#10132 = ORIENTED_EDGE ( 'NONE', *, *, #8085, .T. ) ;
#10133 = CARTESIAN_POINT ( 'NONE',  ( -3.033343224707664820, 3.753672977998667726, -7.249999998634409692 ) ) ;
#10134 = EDGE_CURVE ( 'NONE', #3959, #9532, #6551, .T. ) ;
#10135 = CIRCLE ( 'NONE', #5998, 0.2500000000000002220 ) ;
#10136 = CARTESIAN_POINT ( 'NONE',  ( -115.0000000000000142, -3.122502256758252770E-14, -7.500000000000000000 ) ) ;
#10137 = B_SPLINE_CURVE_WITH_KNOTS ( 'NONE', 3,
 ( #2691, #6433, #14914, #2777, #12627 ),
 .UNSPECIFIED., .F., .F.,
 ( 4, 1, 4 ),
 ( 0.000000000000000000, 0.002309401076758506657, 0.004618802153517013315 ),
 .UNSPECIFIED. ) ;
#10138 = AXIS2_PLACEMENT_3D ( 'NONE', #1101, #8634, #9753 ) ;
#10139 = CARTESIAN_POINT ( 'NONE',  ( 3.535533905932736864, -21.25000000273118772, 3.535533905932738641 ) ) ;
#10140 = UNCERTAINTY_MEASURE_WITH_UNIT (LENGTH_MEASURE( 1.000000000000000082E-05 ), #15799, 'distance_accuracy_value', 'NONE');
#10141 = B_SPLINE_CURVE_WITH_KNOTS ( 'NONE', 3,
 ( #14237, #8107, #746, #15696, #5670, #6889 ),
 .UNSPECIFIED., .F., .F.,
 ( 4, 2, 4 ),
 ( -3.640115492409406142E-06, 0.0002066546034006526487, 0.0004169493222937146744 ),
 .UNSPECIFIED. ) ;
#10142 = CARTESIAN_POINT ( 'NONE',  ( -5.000000000000000000, -30.62500000273118772, -6.123233995736766282E-16 ) ) ;
#10143 = CARTESIAN_POINT ( 'NONE',  ( 0.5711823568785989735, 5.381735091635026613, -2.687499997268816720 ) ) ;
#10144 = CARTESIAN_POINT ( 'NONE',  ( -9.184850993605147944E-16, -23.25000000000000000, 5.000000000000000000 ) ) ;
#10145 = FACE_OUTER_BOUND ( 'NONE', #13672, .T. ) ;
#10146 = CARTESIAN_POINT ( 'NONE',  ( 4.458734124999999437, -21.68750000136559208, 0.000000000000000000 ) ) ;
#10147 = ORIENTED_EDGE ( 'NONE', *, *, #8486, .T. ) ;
#10148 = CARTESIAN_POINT ( 'NONE',  ( 19.99999999999956657, -8.786575603324269439E-13, 1.500000000000000000 ) ) ;
#10149 = CARTESIAN_POINT ( 'NONE',  ( 1.261996585732578113, -4.276409079477644148, -6.562499998634407028 ) ) ;
#10150 = AXIS2_PLACEMENT_3D ( 'NONE', #6308, #13643, #2405 ) ;
#10151 = CARTESIAN_POINT ( 'NONE',  ( -54.99999999999999289, -25.00000000000000000, 17.50000000000000000 ) ) ;
#10152 = EDGE_LOOP ( 'NONE', ( #10057, #1505, #5714, #6332 ) ) ;
#10153 = ORIENTED_EDGE ( 'NONE', *, *, #7861, .F. ) ;
#10154 = VERTEX_POINT ( 'NONE', #15287 ) ;
#10155 = CARTESIAN_POINT ( 'NONE',  ( -4.000000000000000000, -2.309401076758512694, -3.433295621305382461 ) ) ;
#10156 = EDGE_CURVE ( 'NONE', #7077, #2517, #9641, .T. ) ;
#10157 = CARTESIAN_POINT ( 'NONE',  ( -19.99999999999956657, -13.00000000000000178, 2.500000000000877520 ) ) ;
#10158 = EDGE_CURVE ( 'NONE', #7075, #4036, #814, .T. ) ;
#10159 = DIRECTION ( 'NONE',  ( 0.000000000000000000, -1.000000000000000000, 0.000000000000000000 ) ) ;
#10160 = CARTESIAN_POINT ( 'NONE',  ( 4.631580223510930239, 1.444531747605005878E-11, -0.2579703047231843294 ) ) ;
#10161 = CARTESIAN_POINT ( 'NONE',  ( -0.6169862416622959866, -8.783631307151361867, -7.913704048099982735 ) ) ;
#10162 = B_SPLINE_CURVE_WITH_KNOTS ( 'NONE', 3,
 ( #1577, #10073, #10320, #11589, #7657, #3991 ),
 .UNSPECIFIED., .F., .F.,
 ( 4, 2, 4 ),
 ( 0.002452478801916376308, 0.003676905084148007850, 0.004901331366379639391 ),
 .UNSPECIFIED. ) ;
#10163 = CARTESIAN_POINT ( 'NONE',  ( 2.500000000000000000, -2.357898499370432610, 3.252606517456513302E-15 ) ) ;
#10164 = CARTESIAN_POINT ( 'NONE',  ( 1.415196051561583790, -4.795541693661363958, -7.250000000000002665 ) ) ;
#10165 = CARTESIAN_POINT ( 'NONE',  ( 5.000000000000004441, -2.247904837838113790E-16, -3.045263047592945860 ) ) ;
#10166 = FACE_OUTER_BOUND ( 'NONE', #4847, .T. ) ;
#10167 = CARTESIAN_POINT ( 'NONE',  ( 4.458734125000000326, -22.37500000136559564, -1.846868145590734978 ) ) ;
#10168 = CARTESIAN_POINT ( 'NONE',  ( 3.753672977998667726, 3.033343224707664376, -6.499999998634407916 ) ) ;
#10169 = ORIENTED_EDGE ( 'NONE', *, *, #8907, .T. ) ;
#10170 = CARTESIAN_POINT ( 'NONE',  ( 7.500000000000000000, 4.330127018922190096, -7.422398894150031623 ) ) ;
#10171 = B_SPLINE_CURVE_WITH_KNOTS ( 'NONE', 3,
 ( #4685, #9689, #1284, #14629, #3546, #10988, #9610, #8424 ),
 .UNSPECIFIED., .F., .F.,
 ( 4, 2, 2, 4 ),
 ( 2.465131517390770070E-07, 0.001183067374689869946, 0.001774477805458935659, 0.002365888236228001588 ),
 .UNSPECIFIED. ) ;
#10172 = ORIENTED_EDGE ( 'NONE', *, *, #7136, .T. ) ;
#10173 = EDGE_LOOP ( 'NONE', ( #1972, #15450, #1733, #906 ) ) ;
#10174 = CARTESIAN_POINT ( 'NONE',  ( -3.152801135295367096, -30.31250000136559564, -3.152801135295367541 ) ) ;
#10175 = EDGE_CURVE ( 'NONE', #12753, #7038, #10671, .T. ) ;
#10176 = DIRECTION ( 'NONE',  ( 1.000000000000000000, 0.000000000000000000, 0.000000000000000000 ) ) ;
#10177 = EDGE_CURVE ( 'NONE', #5996, #7857, #11579, .T. ) ;
#10178 = EDGE_LOOP ( 'NONE', ( #6833, #9417, #6811, #8667 ) ) ;
#10179 =( GEOMETRIC_REPRESENTATION_CONTEXT ( 3 ) GLOBAL_UNCERTAINTY_ASSIGNED_CONTEXT ( ( #12702 ) ) GLOBAL_UNIT_ASSIGNED_CONTEXT ( ( #6481, #3057, #5101 ) ) REPRESENTATION_CONTEXT ( 'NONE', 'WORKASPACE' ) );
#10180 = CARTESIAN_POINT ( 'NONE',  ( -5.000000000000000000, -28.50000000000000000, -6.123233995736766282E-16 ) ) ;
#10181 =( BOUNDED_CURVE ( )  B_SPLINE_CURVE ( 2, ( #6060, #5820, #8503, #12181, #13313 ),
 .UNSPECIFIED., .F., .F. ) 
 B_SPLINE_CURVE_WITH_KNOTS ( ( 3, 2, 3 ),
 ( 0.9750000000000001998, 0.9875000000000001554, 1.000000000000000000 ),
 .UNSPECIFIED. ) 
 CURVE ( )  GEOMETRIC_REPRESENTATION_ITEM ( )  RATIONAL_B_SPLINE_CURVE ( ( 0.9999999999999986677, 0.9238795325112880708, 1.000000000000000000, 0.9238795325112867385, 1.000000000000000000 ) ) 
 REPRESENTATION_ITEM ( '' )  );
#10182 = CARTESIAN_POINT ( 'NONE',  ( 19.99999999999956657, -8.786575603324269439E-13, -11.50000000000000000 ) ) ;
#10183 = CARTESIAN_POINT ( 'NONE',  ( 3.033343224707661712, -3.753672977998669502, -2.499999998634408804 ) ) ;
#10184 = DIRECTION ( 'NONE',  ( 0.000000000000000000, 0.000000000000000000, -1.000000000000000000 ) ) ;
#10185 = CARTESIAN_POINT ( 'NONE',  ( 2.071067811865475505, -30.81250000000000000, -5.000000000000000888 ) ) ;
#10186 = CARTESIAN_POINT ( 'NONE',  ( -115.0000000000000142, -10.00000000000000888, -7.500000000000000000 ) ) ;
#10187 = DIRECTION ( 'NONE',  ( -1.000000000000000000, 0.000000000000000000, 0.000000000000000000 ) ) ;
#10188 = CARTESIAN_POINT ( 'NONE',  ( -9.184850993605147944E-16, -24.37500000273118772, 5.000000000000000000 ) ) ;
#10189 = FACE_BOUND ( 'NONE', #5994, .T. ) ;
#10190 = AXIS2_PLACEMENT_3D ( 'NONE', #2380, #13691, #2542 ) ;
#10191 = CARTESIAN_POINT ( 'NONE',  ( -4.458734125000000326, -30.87500000136559564, 1.846868145590734089 ) ) ;
#10192 = SURFACE_STYLE_FILL_AREA ( #6397 ) ;
#10193 = ORIENTED_EDGE ( 'NONE', *, *, #11128, .F. ) ;
#10194 = VERTEX_POINT ( 'NONE', #5501 ) ;
#10195 = VECTOR ( 'NONE', #10959, 1000.000000000000114 ) ;
#10197 = ADVANCED_FACE ( 'NONE', ( #4289 ), #12852, .F. ) ;
#10196 = VERTEX_POINT ( 'NONE', #12837 ) ;
#10198 = DIRECTION ( 'NONE',  ( 0.000000000000000000, 1.000000000000000000, 0.000000000000000000 ) ) ;
#10199 = EDGE_CURVE ( 'NONE', #7787, #15426, #7118, .T. ) ;
#10200 = EDGE_LOOP ( 'NONE', ( #14127, #10604, #11451, #10635 ) ) ;
#10201 = DIRECTION ( 'NONE',  ( 0.000000000000000000, 1.000000000000000000, 0.000000000000000000 ) ) ;
#10202 = AXIS2_PLACEMENT_3D ( 'NONE', #13406, #10999, #841 ) ;
#10203 = CARTESIAN_POINT ( 'NONE',  ( 5.000000000000004441, 6.350331166892669572E-15, -1.920263044861758583 ) ) ;
#10204 = AXIS2_PLACEMENT_3D ( 'NONE', #10243, #10159, #465 ) ;
#10205 = DIRECTION ( 'NONE',  ( 0.000000000000000000, -0.000000000000000000, 1.000000000000000000 ) ) ;
#10206 = DIRECTION ( 'NONE',  ( 0.000000000000000000, 0.000000000000000000, -1.000000000000000000 ) ) ;
#10207 = DIRECTION ( 'NONE',  ( -1.000000000000000000, 6.123233995736766036E-17, -6.921730337728899136E-15 ) ) ;
#10208 = CARTESIAN_POINT ( 'NONE',  ( 0.5093500532425063732, 4.799145180956616130, -6.374999998634407028 ) ) ;
#10209 = CARTESIAN_POINT ( 'NONE',  ( 40.98096197215471648, -3.000000000000000000, -26.98110827881998119 ) ) ;
#10210 = VERTEX_POINT ( 'NONE', #7273 ) ;
#10211 = MECHANICAL_DESIGN_GEOMETRIC_PRESENTATION_REPRESENTATION (  '', ( #13021 ), #10972 ) ;
#10212 = CARTESIAN_POINT ( 'NONE',  ( 4.388603409518465170, -3.661800705854443727, -48.61715639207540107 ) ) ;
#10213 = VECTOR ( 'NONE', #3454, 1000.000000000000000 ) ;
#10214 = ORIENTED_EDGE ( 'NONE', *, *, #9375, .T. ) ;
#10215 = CYLINDRICAL_SURFACE ( 'NONE', #1021, 2.499999999999998668 ) ;
#10216 = CARTESIAN_POINT ( 'NONE',  ( 4.458734125000000326, -31.37500000136559564, -1.846868145590734978 ) ) ;
#10217 = ADVANCED_FACE ( 'NONE', ( #4841 ), #3388, .F. ) ;
#10218 = ORIENTED_EDGE ( 'NONE', *, *, #14327, .F. ) ;
#10219 = CARTESIAN_POINT ( 'NONE',  ( -2.131511515620587272, -3.916244202832140253, -6.937499998634407916 ) ) ;
#10220 = CARTESIAN_POINT ( 'NONE',  ( 3.999999999999999112, 1.941961291383486277, -0.3515519931180248192 ) ) ;
#10221 = FACE_BOUND ( 'NONE', #136, .T. ) ;
#10222 = EDGE_CURVE ( 'NONE', #7141, #15429, #2101, .T. ) ;
#10223 = DIRECTION ( 'NONE',  ( 0.000000000000000000, 0.000000000000000000, -1.000000000000000000 ) ) ;
#10224 = AXIS2_PLACEMENT_3D ( 'NONE', #7351, #12105, #8339 ) ;
#10225 = VECTOR ( 'NONE', #7023, 1000.000000000000114 ) ;
#10226 = CARTESIAN_POINT ( 'NONE',  ( 1.415196051561583790, -4.795541693661363958, -5.124999997268817609 ) ) ;
#10227 = CARTESIAN_POINT ( 'NONE',  ( -45.00000000000000000, 0.000000000000000000, 7.500000000000001776 ) ) ;
#10228 =( REPRESENTATION_RELATIONSHIP ('NONE','NONE', #4176, #790 ) REPRESENTATION_RELATIONSHIP_WITH_TRANSFORMATION ( #15476 )SHAPE_REPRESENTATION_RELATIONSHIP( ) );
#10229 = EDGE_CURVE ( 'NONE', #7272, #8967, #10749, .T. ) ;
#10230 = CARTESIAN_POINT ( 'NONE',  ( 5.560781378645575757, 0.000000000000000000, -4.000000000000000000 ) ) ;
#10231 = CARTESIAN_POINT ( 'NONE',  ( -8.190561711645485556E-16, -22.93750000136559564, 4.458734124999999437 ) ) ;
#10232 = ORIENTED_EDGE ( 'NONE', *, *, #6700, .T. ) ;
#10233 = LINE ( 'NONE', #14010, #5109 ) ;
#10234 = CARTESIAN_POINT ( 'NONE',  ( -3.753672977998669946, -3.033343224707661712, -7.749999998634409692 ) ) ;
#10235 = CYLINDRICAL_SURFACE ( 'NONE', #10459, 25.00000000000000000 ) ;
#10236 = ORIENTED_EDGE ( 'NONE', *, *, #1363, .F. ) ;
#10237 = VERTEX_POINT ( 'NONE', #13229 ) ;
#10238 = COLOUR_RGB ( '', 0.08235294, 0.09019608, 0.10196078) ;
#10239 = ORIENTED_EDGE ( 'NONE', *, *, #10899, .F. ) ;
#10240 = DIRECTION ( 'NONE',  ( 0.000000000000000000, 0.000000000000000000, 1.000000000000000000 ) ) ;
#10241 = DIRECTION ( 'NONE',  ( 0.000000000000000000, -0.000000000000000000, -1.000000000000000000 ) ) ;
#10242 = VECTOR ( 'NONE', #1436, 1000.000000000000114 ) ;
#10243 = CARTESIAN_POINT ( 'NONE',  ( -28.86751345948126257, -3.000000000000000000, -50.00000000000000711 ) ) ;
#10244 = CIRCLE ( 'NONE', #3518, 2.000000000000000888 ) ;
#10245 = DIRECTION ( 'NONE',  ( -1.000000000000000000, -0.000000000000000000, -0.000000000000000000 ) ) ;
#10246 = DIRECTION ( 'NONE',  ( -0.000000000000000000, -1.000000000000000000, -0.000000000000000000 ) ) ;
#10247 = PRODUCT_DEFINITION_SHAPE ( 'NONE', 'NONE',  #15994 ) ;
#10248 = CARTESIAN_POINT ( 'NONE',  ( 0.5711823568785989735, 5.381735091635026613, -5.812500000000000000 ) ) ;
#10249 = CARTESIAN_POINT ( 'NONE',  ( 5.200000000000002842, 0.000000000000000000, 0.000000000000000000 ) ) ;
#10250 = ADVANCED_FACE ( 'NONE', ( #4678 ), #15921, .T. ) ;
#10251 = CARTESIAN_POINT ( 'NONE',  ( 67.49999999999931788, 40.00000000000000000, 2.081668171172168513E-14 ) ) ;
#10252 = EDGE_CURVE ( 'NONE', #7219, #5402, #8569, .T. ) ;
#10253 = CARTESIAN_POINT ( 'NONE',  ( -3.152801135295367096, -24.06250000136559564, -3.152801135295367541 ) ) ;
#10254 = LINE ( 'NONE', #9823, #4538 ) ;
#10255 = AXIS2_PLACEMENT_3D ( 'NONE', #1136, #13483, #6077 ) ;
#10256 = CARTESIAN_POINT ( 'NONE',  ( -3.033343224707664376, 3.753672977998667726, -8.249999998634409692 ) ) ;
#10257 = ORIENTED_EDGE ( 'NONE', *, *, #15632, .F. ) ;
#10258 = PLANE ( 'NONE',  #12525 ) ;
#10259 = ORIENTED_EDGE ( 'NONE', *, *, #8812, .T. ) ;
#10260 = ORIENTED_EDGE ( 'NONE', *, *, #1684, .T. ) ;
#10261 = ADVANCED_BREP_SHAPE_REPRESENTATION ( '', ( #9346, #3223 ), #15660 ) ;
#10262 = ORIENTED_EDGE ( 'NONE', *, *, #3035, .T. ) ;
#10263 = CARTESIAN_POINT ( 'NONE',  ( -3.152801135295367985, -30.06250000136559564, 3.152801135295367096 ) ) ;
#10264 = CARTESIAN_POINT ( 'NONE',  ( -2.000000000000006661, 3.464101615137750834, 0.000000000000000000 ) ) ;
#10265 = AXIS2_PLACEMENT_3D ( 'NONE', #9573, #7081, #12066 ) ;
#10266 = EDGE_LOOP ( 'NONE', ( #1348, #3272, #2987 ) ) ;
#10267 = CARTESIAN_POINT ( 'NONE',  ( -0.1750025118121544265, -4.719839900820635314, -3.469254087858253399 ) ) ;
#10268 = DIRECTION ( 'NONE',  ( -0.000000000000000000, 1.000000000000000000, 0.000000000000000000 ) ) ;
#10269 = CARTESIAN_POINT ( 'NONE',  ( -2.131511515620587272, -3.916244202832140253, -2.687499998634407028 ) ) ;
#10270 = CARTESIAN_POINT ( 'NONE',  ( 3.688361877192762428, 2.519395953540043198, -0.3789984458506766574 ) ) ;
#10271 = CARTESIAN_POINT ( 'NONE',  ( 5.000000000000000000, -30.06250000000000000, 2.071067811865478614 ) ) ;
#10272 = CARTESIAN_POINT ( 'NONE',  ( 3.033343224707661712, -3.753672977998669946, -3.499999998634410137 ) ) ;
#10273 = CIRCLE ( 'NONE', #5364, 2.649999999999985700 ) ;
#10274 = DIRECTION ( 'NONE',  ( 0.000000000000000000, 0.000000000000000000, -1.000000000000000000 ) ) ;
#10275 = EDGE_CURVE ( 'NONE', #621, #14429, #5896, .T. ) ;
#10276 = CARTESIAN_POINT ( 'NONE',  ( 5.000000000000000888, -24.06250000273118417, -2.071067811865475505 ) ) ;
#10277 = DIRECTION ( 'NONE',  ( 0.000000000000000000, 1.000000000000000000, 0.000000000000000000 ) ) ;
#10278 = CARTESIAN_POINT ( 'NONE',  ( 2.730187237215162345E-16, -26.18750000136559564, -4.458734124999999437 ) ) ;
#10279 = DIRECTION ( 'NONE',  ( 0.000000000000000000, 0.000000000000000000, -1.000000000000000000 ) ) ;
#10280 = VERTEX_POINT ( 'NONE', #5814 ) ;
#10281 = VERTEX_POINT ( 'NONE', #15686 ) ;
#10282 = CIRCLE ( 'NONE', #9000, 3.499999999999999556 ) ;
#10283 = AXIS2_PLACEMENT_3D ( 'NONE', #9343, #4332, #5857 ) ;
#10284 = EDGE_LOOP ( 'NONE', ( #13309, #5531, #7817, #15748 ) ) ;
#10285 = DIRECTION ( 'NONE',  ( 1.000000000000000000, 0.000000000000000000, 0.000000000000000000 ) ) ;
#10286 =( BOUNDED_CURVE ( )  B_SPLINE_CURVE ( 2, ( #1052, #14715, #2489, #5986, #10911, #12269, #1210, #3710, #15852, #4771, #9696 ),
 .UNSPECIFIED., .F., .F. ) 
 B_SPLINE_CURVE_WITH_KNOTS ( ( 3, 2, 2, 2, 2, 3 ),
 ( 0.2045872658012772849, 0.2124999999999999944, 0.2250000000000000056, 0.2374999999999999889, 0.2500000000000000000, 0.2545872658012772738 ),
 .UNSPECIFIED. ) 
 CURVE ( )  GEOMETRIC_REPRESENTATION_ITEM ( )  RATIONAL_B_SPLINE_CURVE ( ( 0.9646335149384808183, 0.9518143178943438976, 1.000000000000000000, 0.9238795325112867385, 1.000000000000000000, 0.9238795325112867385, 1.000000000000000000, 0.9238795325112867385, 1.000000000000000000, 0.9720652146169430630, 0.9646335149384808183 ) ) 
 REPRESENTATION_ITEM ( '' )  );
#10287 = VERTEX_POINT ( 'NONE', #7347 ) ;
#10288 = CYLINDRICAL_SURFACE ( 'NONE', #5859, 75.00000000000004263 ) ;
#10289 = CIRCLE ( 'NONE', #986, 2.649999999999985700 ) ;
#10290 = CARTESIAN_POINT ( 'NONE',  ( -3.401574460001765221, 4.209348295687701302, -1.562499997268814056 ) ) ;
#10291 = CARTESIAN_POINT ( 'NONE',  ( -4.458734124999999437, -30.18750000136559564, -5.460374474430324690E-16 ) ) ;
#10292 = AXIS2_PLACEMENT_3D ( 'NONE', #15929, #9853, #7280 ) ;
#10293 = DIRECTION ( 'NONE',  ( -1.000000000000000000, 0.000000000000000000, -0.000000000000000000 ) ) ;
#10294 = EDGE_CURVE ( 'NONE', #14193, #6058, #14604, .T. ) ;
#10295 = EDGE_CURVE ( 'NONE', #11118, #4347, #12080, .T. ) ;
#10296 = ADVANCED_FACE ( 'NONE', ( #9680 ), #14618, .T. ) ;
#10297 = ITEM_DEFINED_TRANSFORMATION ( 'NONE', 'NONE', #14827,  #3223 ) ;
#10298 = DIRECTION ( 'NONE',  ( 0.000000000000000000, -1.000000000000000000, 0.000000000000000000 ) ) ;
#10299 = CARTESIAN_POINT ( 'NONE',  ( 2.143131898507869826E-15, 50.00000000000000000, -67.50000000000000000 ) ) ;
#10300 = VERTEX_POINT ( 'NONE', #14861 ) ;
#10301 = VECTOR ( 'NONE', #8294, 1000.000000000000000 ) ;
#10302 = ORIENTED_EDGE ( 'NONE', *, *, #10774, .T. ) ;
#10303 = CARTESIAN_POINT ( 'NONE',  ( -4.795541693661363958, -1.415196051561583790, -1.500000000000001332 ) ) ;
#10304 = CARTESIAN_POINT ( 'NONE',  ( -3.152801135295367985, -30.81250000136559564, 3.152801135295367096 ) ) ;
#10305 = CIRCLE ( 'NONE', #14687, 1.999999999999998224 ) ;
#10306 = VERTEX_POINT ( 'NONE', #4328 ) ;
#10307 = CARTESIAN_POINT ( 'NONE',  ( 2.131511515620586383, 3.916244202832140253, -6.437499998634407028 ) ) ;
#10308 = FACE_OUTER_BOUND ( 'NONE', #6276, .T. ) ;
#10309 = VECTOR ( 'NONE', #14849, 1000.000000000000000 ) ;
#10310 = VECTOR ( 'NONE', #2818, 1000.000000000000000 ) ;
#10311 = CARTESIAN_POINT ( 'NONE',  ( -5.000000000000000000, -28.62500000273118772, -6.123233995736766282E-16 ) ) ;
#10312 = CARTESIAN_POINT ( 'NONE',  ( -4.209348295687703079, -3.401574460001763445, -8.312499997268812280 ) ) ;
#10313 = UNCERTAINTY_MEASURE_WITH_UNIT (LENGTH_MEASURE( 1.000000000000000082E-05 ), #5272, 'distance_accuracy_value', 'NONE');
#10314 = EDGE_CURVE ( 'NONE', #8373, #2474, #2296, .T. ) ;
#10315 = CARTESIAN_POINT ( 'NONE',  ( 4.391654775818395251, -2.390265326283149694, -7.999999997268813168 ) ) ;
#10316 = CARTESIAN_POINT ( 'NONE',  ( -5.000000000000002665, -1.404940523648820476E-14, -8.420263044861757251 ) ) ;
#10317 = CARTESIAN_POINT ( 'NONE',  ( 4.458734124999999437, -22.68750000136559564, 0.000000000000000000 ) ) ;
#10318 = ORIENTED_EDGE ( 'NONE', *, *, #8054, .F. ) ;
#10319 = FACE_OUTER_BOUND ( 'NONE', #460, .T. ) ;
#10320 = CARTESIAN_POINT ( 'NONE',  ( -4.198928548860774157, 0.8158838809860065044, -3.526471437616918170 ) ) ;
#10321 = CARTESIAN_POINT ( 'NONE',  ( -116.3391301858327296, -120.2076149402627294, 7.500000000000001776 ) ) ;
#10322 = VERTEX_POINT ( 'NONE', #15326 ) ;
#10323 = LINE ( 'NONE', #13710, #14179 ) ;
#10324 = ORIENTED_EDGE ( 'NONE', *, *, #10733, .F. ) ;
#10325 = ORIENTED_EDGE ( 'NONE', *, *, #5262, .F. ) ;
#10326 = AXIS2_PLACEMENT_3D ( 'NONE', #9324, #2037, #7293 ) ;
#10327 = CARTESIAN_POINT ( 'NONE',  ( -2.623433461001182465, 7.604994000793860565, -7.633824513837113912 ) ) ;
#10328 = CARTESIAN_POINT ( 'NONE',  ( -2.725741868435985094, 3.045094352034055429, -3.220599429844047012 ) ) ;
#10329 = CARTESIAN_POINT ( 'NONE',  ( 42.02221399786069611, -1.230770033143087371E-15, 1.075528555105620399E-13 ) ) ;
#10330 = CARTESIAN_POINT ( 'NONE',  ( 3.401574460001763445, -4.209348295687703079, -5.187500000000000888 ) ) ;
#10331 = CARTESIAN_POINT ( 'NONE',  ( -6.523606932383977153, -4.893847819345195305, -7.213065638942927293 ) ) ;
#10332 = LINE ( 'NONE', #4168, #11830 ) ;
#10333 = CARTESIAN_POINT ( 'NONE',  ( -3.401574460001764777, 4.209348295687701302, -6.687500000000003553 ) ) ;
#10334 = CARTESIAN_POINT ( 'NONE',  ( 35.00000000000000000, 50.00000000000000000, -2.649999999999985700 ) ) ;
#10335 = FACE_OUTER_BOUND ( 'NONE', #12688, .T. ) ;
#10336 = CARTESIAN_POINT ( 'NONE',  ( -8.190561711645485556E-16, -22.68750000136559564, 4.458734124999999437 ) ) ;
#10337 = CARTESIAN_POINT ( 'NONE',  ( 1.261996585732578113, -4.276409079477644148, -5.812499998634406140 ) ) ;
#10338 = ORIENTED_EDGE ( 'NONE', *, *, #14054, .F. ) ;
#10339 = CARTESIAN_POINT ( 'NONE',  ( 7.703928834700302986, -4.447865386531949738, -7.917997657324739258 ) ) ;
#10340 = ORIENTED_EDGE ( 'NONE', *, *, #7226, .F. ) ;
#10341 = ORIENTED_EDGE ( 'NONE', *, *, #3148, .T. ) ;
#10342 = CARTESIAN_POINT ( 'NONE',  ( 4.458734124999999437, -22.50000000136559208, 1.846868145590737864 ) ) ;
#10343 = CARTESIAN_POINT ( 'NONE',  ( -6.765421556309547668E-13, 50.00000000000000000, 67.49999999999930367 ) ) ;
#10344 = ORIENTED_EDGE ( 'NONE', *, *, #6740, .F. ) ;
#10345 = CARTESIAN_POINT ( 'NONE',  ( 0.5469614295415388128, -4.303013824935362663, -3.535263753543555598 ) ) ;
#10346 = ADVANCED_FACE ( 'NONE', ( #4994 ), #6980, .F. ) ;
#10347 = LINE ( 'NONE', #15274, #9019 ) ;
#10348 = CARTESIAN_POINT ( 'NONE',  ( -3.753672977998669502, -3.033343224707661712, -2.749999998634409248 ) ) ;
#10349 = DIRECTION ( 'NONE',  ( 0.000000000000000000, 0.000000000000000000, 1.000000000000000000 ) ) ;
#10350 = CARTESIAN_POINT ( 'NONE',  ( 2.071067811865475505, -27.81250000000000000, -5.000000000000000888 ) ) ;
#10351 = CARTESIAN_POINT ( 'NONE',  ( -4.276409079477644148, -1.261996585732578335, -2.812499998634407472 ) ) ;
#10352 = CARTESIAN_POINT ( 'NONE',  ( -6.874999999999999112, -4.690970937165712229, -7.298562697733106397 ) ) ;
#10353 = CARTESIAN_POINT ( 'NONE',  ( 2.500000000000000000, 2.357898499370433054, -1.951563910473907981E-15 ) ) ;
#10354 = CARTESIAN_POINT ( 'NONE',  ( 5.000000000000000000, -26.18750000273119127, 2.071067811865478614 ) ) ;
#10355 = LINE ( 'NONE', #2982, #10672 ) ;
#10356 = CARTESIAN_POINT ( 'NONE',  ( -4.458734124999999437, -25.00000000136559564, -1.846868145590735644 ) ) ;
#10357 = DIRECTION ( 'NONE',  ( 0.000000000000000000, -1.000000000000000000, 0.000000000000000000 ) ) ;
#10358 = ORIENTED_EDGE ( 'NONE', *, *, #2998, .T. ) ;
#10359 = ORIENTED_EDGE ( 'NONE', *, *, #6446, .F. ) ;
#10360 = CARTESIAN_POINT ( 'NONE',  ( 1.747541505913279281, -3.837784562140273081, -3.503702292528912299 ) ) ;
#10361 = EDGE_LOOP ( 'NONE', ( #158, #5542, #10214, #6945 ) ) ;
#10362 = ORIENTED_EDGE ( 'NONE', *, *, #9551, .T. ) ;
#10363 = CARTESIAN_POINT ( 'NONE',  ( -35.00000000000000000, 37.00000000000000000, 0.000000000000000000 ) ) ;
#10364 = ADVANCED_FACE ( 'NONE', ( #13633 ), #7977, .F. ) ;
#10365 = EDGE_CURVE ( 'NONE', #3476, #14971, #9284, .T. ) ;
#10366 = FACE_OUTER_BOUND ( 'NONE', #7514, .T. ) ;
#10367 = CARTESIAN_POINT ( 'NONE',  ( -8.190561711645485556E-16, -30.93750000136559564, 4.458734124999999437 ) ) ;
#10368 = CARTESIAN_POINT ( 'NONE',  ( 0.000000000000000000, 20.00000000000000000, 5.000000000000000000 ) ) ;
#10369 = CONTEXT_DEPENDENT_SHAPE_REPRESENTATION ( #3104, #15719 ) ;
#10370 = CARTESIAN_POINT ( 'NONE',  ( -1.261996585732579224, 4.276409079477648589, -8.312499998634407916 ) ) ;
#10371 = CARTESIAN_POINT ( 'NONE',  ( 3.753672977998667726, 3.033343224707664376, 0.5000000013655936382 ) ) ;
#10372 = ORIENTED_EDGE ( 'NONE', *, *, #1363, .T. ) ;
#10373 = APPLICATION_PROTOCOL_DEFINITION ( 'draft international standard', 'automotive_design', 1998, #9798 ) ;
#10374 = VERTEX_POINT ( 'NONE', #161 ) ;
#10375 = B_SPLINE_CURVE_WITH_KNOTS ( 'NONE', 3,
 ( #4852, #13398, #6061, #14710, #2337, #8577 ),
 .UNSPECIFIED., .F., .F.,
 ( 4, 2, 4 ),
 ( 0.000000000000000000, 0.0002095117440854730670, 0.0004190234881709461339 ),
 .UNSPECIFIED. ) ;
#10376 = DIRECTION ( 'NONE',  ( 0.000000000000000000, 1.000000000000000000, 0.000000000000000000 ) ) ;
#10377 = CARTESIAN_POINT ( 'NONE',  ( -1.846868145590737420, -28.75000000136559208, 4.458734124999999437 ) ) ;
#10378 = VERTEX_POINT ( 'NONE', #6593 ) ;
#10379 = EDGE_CURVE ( 'NONE', #6271, #13973, #10323, .T. ) ;
#10380 = ADVANCED_FACE ( 'NONE', ( #11664 ), #459, .T. ) ;
#10381 = FILL_AREA_STYLE ('',( #14252 ) ) ;
#10382 = VECTOR ( 'NONE', #822, 1000.000000000000000 ) ;
#10383 = CARTESIAN_POINT ( 'NONE',  ( 4.795541693661363958, 1.415196051561583790, -6.874999997268815832 ) ) ;
#10384 = DIRECTION ( 'NONE',  ( -0.5000000000000005551, 0.000000000000000000, 0.8660254037844382635 ) ) ;
#10385 = DIRECTION ( 'NONE',  ( 0.000000000000000000, 0.000000000000000000, -1.000000000000000000 ) ) ;
#10386 = VERTEX_POINT ( 'NONE', #1814 ) ;
#10387 = PLANE ( 'NONE',  #3318 ) ;
#10388 = CARTESIAN_POINT ( 'NONE',  ( 4.276409079477644148, 1.261996585732577891, -7.312499998634407916 ) ) ;
#10389 = CARTESIAN_POINT ( 'NONE',  ( 30.02221399786053979, -35.00000000000000000, -15.99999999999998579 ) ) ;
#10390 = ORIENTED_EDGE ( 'NONE', *, *, #183, .F. ) ;
#10391 = DIRECTION ( 'NONE',  ( 1.000000000000000000, 0.000000000000000000, 0.000000000000000000 ) ) ;
#10392 = ORIENTED_EDGE ( 'NONE', *, *, #15255, .F. ) ;
#10393 = ORIENTED_EDGE ( 'NONE', *, *, #9869, .T. ) ;
#10394 = CARTESIAN_POINT ( 'NONE',  ( 3.401574460001763445, -4.209348295687703079, -0.1875000000000048572 ) ) ;
#10395 = EDGE_CURVE ( 'NONE', #739, #13808, #3087, .T. ) ;
#10396 = CARTESIAN_POINT ( 'NONE',  ( -3.522875095019672109, 2.820352903225427532, -3.598441714920591394 ) ) ;
#10397 = EDGE_CURVE ( 'NONE', #6220, #11087, #6713, .T. ) ;
#10398 = CARTESIAN_POINT ( 'NONE',  ( 25.00000000000000000, 2.789133085058098087E-16, -2.055000000000000160 ) ) ;
#10399 = CARTESIAN_POINT ( 'NONE',  ( 2.500000000000000000, 1.178949249685218525, 2.041999999999999371 ) ) ;
#10400 = CYLINDRICAL_SURFACE ( 'NONE', #347, 40.00000000000001421 ) ;
#10401 = CARTESIAN_POINT ( 'NONE',  ( 0.000000000000000000, -20.00000000000000000, 0.000000000000000000 ) ) ;
#10402 = AXIS2_PLACEMENT_3D ( 'NONE', #9078, #15375, #15051 ) ;
#10403 = DIRECTION ( 'NONE',  ( 1.000000000000000000, 0.000000000000000000, 0.000000000000000000 ) ) ;
#10404 = CARTESIAN_POINT ( 'NONE',  ( 4.795541693661363958, 1.415196051561583790, -8.000000000000003553 ) ) ;
#10405 = CARTESIAN_POINT ( 'NONE',  ( -1.846868145590734756, -23.12500000136559564, -4.458734125000000326 ) ) ;
#10406 = CARTESIAN_POINT ( 'NONE',  ( 3.916244202832140253, -2.131511515620588160, -7.687499998634407916 ) ) ;
#10407 = ORIENTED_EDGE ( 'NONE', *, *, #3610, .F. ) ;
#10408 = CARTESIAN_POINT ( 'NONE',  ( 4.000000000000000000, 0.000000000000000000, 0.000000000000000000 ) ) ;
#10409 = ORIENTED_EDGE ( 'NONE', *, *, #13696, .F. ) ;
#10410 = ORIENTED_EDGE ( 'NONE', *, *, #402, .F. ) ;
#10411 = PRODUCT_DEFINITION_SHAPE ( 'NONE', 'NONE',  #2153 ) ;
#10412 = CARTESIAN_POINT ( 'NONE',  ( -3.152801135295367985, -21.81250000136559208, 3.152801135295367096 ) ) ;
#10413 = CARTESIAN_POINT ( 'NONE',  ( 2.171643655288379993, -3.365003104552334978, -1.195831703456429434E-14 ) ) ;
#10414 = EDGE_CURVE ( 'NONE', #757, #5100, #14951, .T. ) ;
#10415 = VERTEX_POINT ( 'NONE', #15404 ) ;
#10416 = VECTOR ( 'NONE', #1290, 1000.000000000000000 ) ;
#10417 = CARTESIAN_POINT ( 'NONE',  ( 2.500000000000000000, 2.357898499370433054, -1.951563910473907981E-15 ) ) ;
#10418 = CARTESIAN_POINT ( 'NONE',  ( 2.143131898507869826E-15, 37.00000000000000000, -67.50000000000000000 ) ) ;
#10419 = CARTESIAN_POINT ( 'NONE',  ( -4.799145180956616130, 0.5093500532425063732, -3.874999998634404363 ) ) ;
#10420 = CARTESIAN_POINT ( 'NONE',  ( -35.00000000000000000, 37.00000000000000000, 2.649999999999992806 ) ) ;
#10421 = CARTESIAN_POINT ( 'NONE',  ( -2.071067811865478170, -25.31250000000000000, 5.000000000000000000 ) ) ;
#10422 = CARTESIAN_POINT ( 'NONE',  ( 4.799145180956616130, -0.5093500532425063732, -7.374999998634408804 ) ) ;
#10423 = CARTESIAN_POINT ( 'NONE',  ( -43.89752705808261624, -2.999999999999999556, -21.87149547239932090 ) ) ;
#10424 = DIRECTION ( 'NONE',  ( 0.000000000000000000, 1.000000000000000000, 0.000000000000000000 ) ) ;
#10425 = CARTESIAN_POINT ( 'NONE',  ( -9.184850993605147944E-16, -26.37500000273118417, 5.000000000000000000 ) ) ;
#10426 = DIRECTION ( 'NONE',  ( 0.000000000000000000, 0.000000000000000000, -1.000000000000000000 ) ) ;
#10427 = CARTESIAN_POINT ( 'NONE',  ( -4.458734124999999437, -27.00000000136559564, -1.846868145590735644 ) ) ;
#10428 = EDGE_CURVE ( 'NONE', #15817, #9981, #12789, .T. ) ;
#10429 = CARTESIAN_POINT ( 'NONE',  ( 2.352174619734370697, -7.302225387959956571, -7.450218641349208859 ) ) ;
#10430 = ORIENTED_EDGE ( 'NONE', *, *, #9790, .F. ) ;
#10431 = ORIENTED_EDGE ( 'NONE', *, *, #15217, .T. ) ;
#10432 = CIRCLE ( 'NONE', #3444, 2.000000000000001776 ) ;
#10433 = CARTESIAN_POINT ( 'NONE',  ( -6.473970235329672780E-16, -4.862606272033106691, -3.745885042887442395 ) ) ;
#10434 = EDGE_LOOP ( 'NONE', ( #7616, #8964, #7158, #7533 ) ) ;
#10435 = DIRECTION ( 'NONE',  ( -1.000000000000000000, -0.000000000000000000, -0.000000000000000000 ) ) ;
#10436 = ORIENTED_EDGE ( 'NONE', *, *, #2079, .F. ) ;
#10437 = CARTESIAN_POINT ( 'NONE',  ( -21.01110699893060030, -1.230770033143087371E-15, 36.39230484541324273 ) ) ;
#10438 = CARTESIAN_POINT ( 'NONE',  ( 0.5711823568785988625, 5.381735091635026613, -1.687499997268816054 ) ) ;
#10439 = CARTESIAN_POINT ( 'NONE',  ( -3.152801135295367985, -29.06250000136559564, 3.152801135295367096 ) ) ;
#10440 = PRESENTATION_LAYER_ASSIGNMENT (  '', '', ( #3967 ) ) ;
#10441 = CARTESIAN_POINT ( 'NONE',  ( -5.000000000000004441, -7.530481206757679743E-15, -1.420263044861758361 ) ) ;
#10442 = CARTESIAN_POINT ( 'NONE',  ( -24.26932219902320043, 37.00000000000000000, 5.999999999999998224 ) ) ;
#10443 = ITEM_DEFINED_TRANSFORMATION ( 'NONE', 'NONE', #10190,  #3223 ) ;
#10444 = AXIS2_PLACEMENT_3D ( 'NONE', #4513, #4367, #11696 ) ;
#10445 = CARTESIAN_POINT ( 'NONE',  ( 1.250000000000000444, -7.938566201357367902, -7.198902722707432034 ) ) ;
#10446 = CARTESIAN_POINT ( 'NONE',  ( -4.276409079477644148, -1.261996585732578335, -0.06249999863440838799 ) ) ;
#10447 = EDGE_CURVE ( 'NONE', #13350, #11846, #4110, .T. ) ;
#10449 = ADVANCED_FACE ( 'NONE', ( #8806 ), #5461, .F. ) ;
#10448 = VERTEX_POINT ( 'NONE', #7515 ) ;
#10450 = ORIENTED_EDGE ( 'NONE', *, *, #2365, .T. ) ;
#10451 = CARTESIAN_POINT ( 'NONE',  ( 31.75426480542940766, 0.000000000000000000, 15.00000000000001066 ) ) ;
#10452 = AXIS2_PLACEMENT_3D ( 'NONE', #3813, #9953, #7628 ) ;
#10453 = VERTEX_POINT ( 'NONE', #11974 ) ;
#10454 = CONTEXT_DEPENDENT_SHAPE_REPRESENTATION ( #11864, #11648 ) ;
#10455 = CIRCLE ( 'NONE', #10204, 28.00000000000000355 ) ;
#10456 = CARTESIAN_POINT ( 'NONE',  ( 5.000000000000093259, 0.7223674278660628945, -5.021799365517154001 ) ) ;
#10457 = DIRECTION ( 'NONE',  ( 0.000000000000000000, 0.000000000000000000, 1.000000000000000000 ) ) ;
#10458 = LINE ( 'NONE', #15392, #10772 ) ;
#10459 = AXIS2_PLACEMENT_3D ( 'NONE', #1650, #13186, #1970 ) ;
#10460 = VECTOR ( 'NONE', #3569, 1000.000000000000000 ) ;
#10461 = CARTESIAN_POINT ( 'NONE',  ( -1.415196051561583790, 4.795541693661363958, -8.624999997268814056 ) ) ;
#10462 = CARTESIAN_POINT ( 'NONE',  ( 67.49999999999931788, 37.00000000000000000, 2.081668171172168513E-14 ) ) ;
#10463 = CARTESIAN_POINT ( 'NONE',  ( -4.391654775818395251, 2.390265326283148806, -1.625000000000001332 ) ) ;
#10464 = LINE ( 'NONE', #9261, #9676 ) ;
#10465 = EDGE_CURVE ( 'NONE', #7938, #6661, #9416, .T. ) ;
#10466 = VERTEX_POINT ( 'NONE', #13262 ) ;
#10467 = PRESENTATION_LAYER_ASSIGNMENT (  '', '', ( #1420 ) ) ;
#10468 = CARTESIAN_POINT ( 'NONE',  ( 7.500000000000002665, 3.639598441879749124, -0.7155132341745285007 ) ) ;
#10469 = CARTESIAN_POINT ( 'NONE',  ( -7.549004593702457022, 4.358419834287859729, -7.700121441565834779 ) ) ;
#10470 = CARTESIAN_POINT ( 'NONE',  ( -5.000000000000000000, -26.62500000273118772, -6.123233995736766282E-16 ) ) ;
#10471 = EDGE_LOOP ( 'NONE', ( #15782, #11881, #8568, #1679 ) ) ;
#10472 = CARTESIAN_POINT ( 'NONE',  ( 43.08845726811992449, -5.000000000000000000, -38.63139720814411504 ) ) ;
#10473 = ORIENTED_EDGE ( 'NONE', *, *, #14528, .T. ) ;
#10474 = ORIENTED_EDGE ( 'NONE', *, *, #8019, .F. ) ;
#10475 = CARTESIAN_POINT ( 'NONE',  ( -9.184850993605147944E-16, -30.25000000000000000, 5.000000000000000000 ) ) ;
#10476 = DIRECTION ( 'NONE',  ( -0.000000000000000000, 1.000000000000000000, -0.000000000000000000 ) ) ;
#10477 = CIRCLE ( 'NONE', #8157, 0.2500000000000002220 ) ;
#10478 = FACE_OUTER_BOUND ( 'NONE', #6557, .T. ) ;
#10479 = VECTOR ( 'NONE', #5506, 1000.000000000000000 ) ;
#10480 = VECTOR ( 'NONE', #8573, 1000.000000000000000 ) ;
#10481 = CARTESIAN_POINT ( 'NONE',  ( 3.535533905932738197, -26.00000000273118417, -3.535533905932738197 ) ) ;
#10482 = CARTESIAN_POINT ( 'NONE',  ( 7.500000000000000000, 4.330127018922190096, -7.422398894150031623 ) ) ;
#10483 = DIRECTION ( 'NONE',  ( -0.000000000000000000, -1.000000000000000000, -0.000000000000000000 ) ) ;
#10484 = CYLINDRICAL_SURFACE ( 'NONE', #13864, 2.000000000000001776 ) ;
#10485 = CARTESIAN_POINT ( 'NONE',  ( -43.99999999999978684, -11.00000000000000178, 1.499999999999998668 ) ) ;
#10486 = ADVANCED_FACE ( 'NONE', ( #4560 ), #3270, .F. ) ;
#10487 = DIRECTION ( 'NONE',  ( -1.000000000000000000, -0.000000000000000000, -0.000000000000000000 ) ) ;
#10488 = ADVANCED_FACE ( 'NONE', ( #9637 ), #1890, .F. ) ;
#10489 = CARTESIAN_POINT ( 'NONE',  ( 1.846868145590736310, -24.62500000136559564, 4.458734124999999437 ) ) ;
#10490 = EDGE_CURVE ( 'NONE', #3781, #8839, #269, .T. ) ;
#10491 = ADVANCED_FACE ( 'NONE', ( #4482 ), #10786, .T. ) ;
#10492 = CARTESIAN_POINT ( 'NONE',  ( 3.033343224707661712, -3.753672977998669946, -0.4999999986344072500 ) ) ;
#10493 = ORIENTED_EDGE ( 'NONE', *, *, #4821, .F. ) ;
#10494 = TOROIDAL_SURFACE ( 'NONE', #8434, 4.000000000000000000, 0.2500000000000000000 ) ;
#10495 = CARTESIAN_POINT ( 'NONE',  ( -34.99999999999999289, -11.00000000000000178, 2.000000000000830447 ) ) ;
#10496 = ORIENTED_EDGE ( 'NONE', *, *, #4821, .T. ) ;
#10497 = EDGE_LOOP ( 'NONE', ( #5427, #7042, #11393, #11133 ) ) ;
#10498 = AXIS2_PLACEMENT_3D ( 'NONE', #10882, #4822, #2383 ) ;
#10499 =( LENGTH_UNIT ( ) NAMED_UNIT ( * ) SI_UNIT ( .MILLI., .METRE. ) );
#10500 = CARTESIAN_POINT ( 'NONE',  ( 3.152801135295367541, -25.56250000136559564, -3.152801135295367541 ) ) ;
#10501 = CARTESIAN_POINT ( 'NONE',  ( 30.02221399786059663, 1.999999999999998224, -16.00000000000007461 ) ) ;
#10502 = ORIENTED_EDGE ( 'NONE', *, *, #11885, .T. ) ;
#10503 = LINE ( 'NONE', #15515, #13817 ) ;
#10504 = AXIS2_PLACEMENT_3D ( 'NONE', #3188, #1810, #5693 ) ;
#10505 = CARTESIAN_POINT ( 'NONE',  ( 7.500000000000000000, -3.202733125952097915, -7.213074474937297254 ) ) ;
#10506 = CARTESIAN_POINT ( 'NONE',  ( 4.276409079477644148, 1.261996585732577891, -4.312499998634405252 ) ) ;
#10507 = CARTESIAN_POINT ( 'NONE',  ( 5.000000000000093259, 0.7223674278660628945, -5.896799362785968945 ) ) ;
#10508 = CIRCLE ( 'NONE', #12288, 2.041999999999999815 ) ;
#10509 = CARTESIAN_POINT ( 'NONE',  ( -5.000000000000000888, -24.43750000000000355, 2.071067811865474617 ) ) ;
#10510 = CLOSED_SHELL ( 'NONE', ( #15160, #2643, #1345, #12931, #7187, #11149, #13015, #7540, #15670, #10364, #14424, #15472, #10608, #11147, #12206, #14486, #3236, #13570, #5630, #1509, #11814, #6096, #2384, #9870, #7685, #4962, #7922, #10666, #13304, #4844, #2663, #1895, #4069, #1859, #9833, #9236, #11283, #15862, #8089, #1842, #4336, #11506, #5379, #1839, #1681, #12047, #519, #9502, #9069, #381, #12720, #14031, #10736, #13076 ) ) ;
#10511 = CARTESIAN_POINT ( 'NONE',  ( -3.033343224707664376, 3.753672977998667726, -6.999999998634408804 ) ) ;
#10512 = DIRECTION ( 'NONE',  ( 0.000000000000000000, 0.000000000000000000, 1.000000000000000000 ) ) ;
#10513 = CARTESIAN_POINT ( 'NONE',  ( 0.000000000000000000, 0.000000000000000000, 0.000000000000000000 ) ) ;
#10514 = CARTESIAN_POINT ( 'NONE',  ( -5.000000000000000000, -24.62500000273118417, -6.123233995736766282E-16 ) ) ;
#10515 = ADVANCED_FACE ( 'NONE', ( #7156 ), #13117, .T. ) ;
#10516 = VERTEX_POINT ( 'NONE', #14343 ) ;
#10517 = CARTESIAN_POINT ( 'NONE',  ( 4.458734124999997661, -24.50000000136559564, 1.846868145590737864 ) ) ;
#10518 = DIRECTION ( 'NONE',  ( 0.000000000000000000, 0.000000000000000000, -1.000000000000000000 ) ) ;
#10519 = VERTEX_POINT ( 'NONE', #10562 ) ;
#10520 = ORIENTED_EDGE ( 'NONE', *, *, #3648, .T. ) ;
#10521 = CARTESIAN_POINT ( 'NONE',  ( 7.500000000000000888, -0.7512838658081425480, 1.521271173268723212E-15 ) ) ;
#10522 = CARTESIAN_POINT ( 'NONE',  ( 0.000000000000000000, -20.00000000000000000, 0.000000000000000000 ) ) ;
#10523 = CARTESIAN_POINT ( 'NONE',  ( -3.916244202832140253, 2.131511515620587272, -2.937499998634407472 ) ) ;
#10524 = ORIENTED_EDGE ( 'NONE', *, *, #4976, .F. ) ;
#10525 = CARTESIAN_POINT ( 'NONE',  ( -39.99999999999999289, -11.00000000000000178, 8.300651832549021947E-13 ) ) ;
#10526 = VECTOR ( 'NONE', #1803, 1000.000000000000000 ) ;
#10527 = CARTESIAN_POINT ( 'NONE',  ( 40.12140847263850674, -3.395032785697077671, -27.89299687554618856 ) ) ;
#10528 = CARTESIAN_POINT ( 'NONE',  ( 2.730187237215162345E-16, -28.43750000136559564, -4.458734124999999437 ) ) ;
#10529 = DIRECTION ( 'NONE',  ( 0.000000000000000000, 1.000000000000000000, 0.000000000000000000 ) ) ;
#10530 = CARTESIAN_POINT ( 'NONE',  ( 4.999999999999848121, -1.272547481429015859, -4.086597482644646284 ) ) ;
#10531 = AXIS2_PLACEMENT_3D ( 'NONE', #7742, #220, #12553 ) ;
#10532 = CARTESIAN_POINT ( 'NONE',  ( 0.5711823568785988625, 5.381735091635026613, -7.687499997268817609 ) ) ;
#10533 = CARTESIAN_POINT ( 'NONE',  ( -7.500000000000005329, 4.330127018922194537, -0.9999999999999974465 ) ) ;
#10534 = ORIENTED_EDGE ( 'NONE', *, *, #13971, .F. ) ;
#10535 =( NAMED_UNIT ( * ) SI_UNIT ( $, .STERADIAN. ) SOLID_ANGLE_UNIT ( ) );
#10536 = VECTOR ( 'NONE', #2979, 1000.000000000000000 ) ;
#10537 = ORIENTED_EDGE ( 'NONE', *, *, #14054, .T. ) ;
#10538 = CARTESIAN_POINT ( 'NONE',  ( -4.000000000000000000, 0.000000000000000000, 0.000000000000000000 ) ) ;
#10539 = AXIS2_PLACEMENT_3D ( 'NONE', #4710, #13664, #5358 ) ;
#10540 = ORIENTED_EDGE ( 'NONE', *, *, #8418, .T. ) ;
#10541 = CONTEXT_DEPENDENT_SHAPE_REPRESENTATION ( #11348, #4938 ) ;
#10542 =( REPRESENTATION_RELATIONSHIP ('NONE','NONE', #4176, #279 ) REPRESENTATION_RELATIONSHIP_WITH_TRANSFORMATION ( #6501 )SHAPE_REPRESENTATION_RELATIONSHIP( ) );
#10543 = CIRCLE ( 'NONE', #3062, 5.000000000000000888 ) ;
#10544 = DIRECTION ( 'NONE',  ( -0.000000000000000000, -0.000000000000000000, -1.000000000000000000 ) ) ;
#10545 = ADVANCED_FACE ( 'NONE', ( #11741 ), #15729, .T. ) ;
#10546 = ADVANCED_FACE ( 'NONE', ( #9340 ), #1005, .F. ) ;
#10547 = CARTESIAN_POINT ( 'NONE',  ( 39.58615490320391217, -4.472255266398825313, 28.43259952176492433 ) ) ;
#10548 =( GEOMETRIC_REPRESENTATION_CONTEXT ( 3 ) GLOBAL_UNCERTAINTY_ASSIGNED_CONTEXT ( ( #4179 ) ) GLOBAL_UNIT_ASSIGNED_CONTEXT ( ( #14586, #14673, #6027 ) ) REPRESENTATION_CONTEXT ( 'NONE', 'WORKASPACE' ) );
#10549 = DIRECTION ( 'NONE',  ( 0.000000000000000000, 0.000000000000000000, 1.000000000000000000 ) ) ;
#10550 = AXIS2_PLACEMENT_3D ( 'NONE', #3729, #1472, #8764 ) ;
#10551 = PRODUCT ( 'Precision Linear Jaw Guides', 'Precision Linear Jaw Guides', '', ( #5676 ) ) ;
#10552 = CARTESIAN_POINT ( 'NONE',  ( 0.5711823568785989735, 5.381735091635026613, -8.687499997268814056 ) ) ;
#10553 = CARTESIAN_POINT ( 'NONE',  ( -39.99999999999999289, -11.00000000000000178, 2.500000000001739497 ) ) ;
#10554 = CARTESIAN_POINT ( 'NONE',  ( -4.203833317240879275, -1.627343821129593859, -3.597273115243890818 ) ) ;
#10555 = LINE ( 'NONE', #9409, #3225 ) ;
#10556 = VERTEX_POINT ( 'NONE', #15643 ) ;
#10557 = CARTESIAN_POINT ( 'NONE',  ( -35.00000000000000000, 37.00000000000000000, 0.000000000000000000 ) ) ;
#10558 = DIRECTION ( 'NONE',  ( -1.000000000000000000, -0.000000000000000000, -0.000000000000000000 ) ) ;
#10559 = AXIS2_PLACEMENT_3D ( 'NONE', #11964, #10776, #4629 ) ;
#10560 = DIRECTION ( 'NONE',  ( -0.000000000000000000, -0.000000000000000000, 1.000000000000000000 ) ) ;
#10561 = VERTEX_POINT ( 'NONE', #14426 ) ;
#10562 = CARTESIAN_POINT ( 'NONE',  ( 5.384454397937118664, 0.000000000000000000, -5.000000000000000000 ) ) ;
#10563 = ORIENTED_EDGE ( 'NONE', *, *, #2734, .F. ) ;
#10564 = VERTEX_POINT ( 'NONE', #9568 ) ;
#10565 = FACE_OUTER_BOUND ( 'NONE', #3207, .T. ) ;
#10566 = CARTESIAN_POINT ( 'NONE',  ( -4.141042297810615835, 2.227970268150415656, -3.687027686973619822 ) ) ;
#10567 = B_SPLINE_CURVE_WITH_KNOTS ( 'NONE', 3,
 ( #2417, #96, #7369, #11156, #12278, #8665 ),
 .UNSPECIFIED., .F., .F.,
 ( 4, 2, 4 ),
 ( 0.002365888236227977302, 0.003551327329835078910, 0.004736766423442180518 ),
 .UNSPECIFIED. ) ;
#10568 = AXIS2_PLACEMENT_3D ( 'NONE', #9134, #6865, #6782 ) ;
#10569 = CARTESIAN_POINT ( 'NONE',  ( -150.5560796608385203, -71.58493649053927754, 7.500000000000001776 ) ) ;
#10570 = EDGE_CURVE ( 'NONE', #12914, #11431, #6832, .T. ) ;
#10571 = ADVANCED_FACE ( 'NONE', ( #4715 ), #13188, .T. ) ;
#10572 = AXIS2_PLACEMENT_3D ( 'NONE', #4908, #881, #5799 ) ;
#10573 = DIRECTION ( 'NONE',  ( 1.000000000000000000, 0.000000000000000000, 0.000000000000000000 ) ) ;
#10574 = CARTESIAN_POINT ( 'NONE',  ( -3.535533905932738641, -25.37500000000000000, 3.535533905932737309 ) ) ;
#10575 = CARTESIAN_POINT ( 'NONE',  ( -7.500000000000001776, -4.330127018922197202, -7.564335161054499324 ) ) ;
#10576 = DIRECTION ( 'NONE',  ( -0.000000000000000000, 1.000000000000000000, -0.000000000000000000 ) ) ;
#10577 = CARTESIAN_POINT ( 'NONE',  ( -17.99999999999979394, -11.00000000000000178, 3.499999999999998668 ) ) ;
#10578 = CARTESIAN_POINT ( 'NONE',  ( 2.500000000000000000, -1.178949249685213863, 2.042000000000002924 ) ) ;
#10579 = CARTESIAN_POINT ( 'NONE',  ( -4.458734124999999437, -28.18750000136559564, -5.460374474430324690E-16 ) ) ;
#10580 = CARTESIAN_POINT ( 'NONE',  ( 0.5093500532425063732, 4.799145180956616130, -1.124999998634405918 ) ) ;
#10581 = VERTEX_POINT ( 'NONE', #8057 ) ;
#10582 = VECTOR ( 'NONE', #11573, 1000.000000000000000 ) ;
#10583 = DIRECTION ( 'NONE',  ( -0.000000000000000000, 1.000000000000000000, -0.000000000000000000 ) ) ;
#10584 = ORIENTED_EDGE ( 'NONE', *, *, #12912, .F. ) ;
#10585 = ORIENTED_EDGE ( 'NONE', *, *, #14247, .F. ) ;
#10586 = CARTESIAN_POINT ( 'NONE',  ( -8.190561711645485556E-16, -27.93750000136559564, 4.458734124999999437 ) ) ;
#10587 = B_SPLINE_CURVE_WITH_KNOTS ( 'NONE', 3,
 ( #3245, #13008, #10445, #1946, #4214, #12686, #6894, #5677, #9242 ),
 .UNSPECIFIED., .F., .F.,
 ( 4, 2, 1, 2, 4 ),
 ( 0.000000000000000000, 0.002165063509461099666, 0.004330127018922197597, 0.006495190528383295095, 0.008660254037844393460 ),
 .UNSPECIFIED. ) ;
#10588 = CARTESIAN_POINT ( 'NONE',  ( -6.473970235329672780E-16, -4.862606272033106691, -3.745885042887442395 ) ) ;
#10589 = CYLINDRICAL_SURFACE ( 'NONE', #12267, 5.000000000000000000 ) ;
#10590 = EDGE_CURVE ( 'NONE', #14037, #8368, #880, .T. ) ;
#10591 = ADVANCED_FACE ( 'NONE', ( #4953 ), #4797, .T. ) ;
#10592 = DIRECTION ( 'NONE',  ( 0.000000000000000000, 0.000000000000000000, -1.000000000000000000 ) ) ;
#10593 = CARTESIAN_POINT ( 'NONE',  ( 3.916244202832140253, -2.131511515620588160, -4.437499998634405252 ) ) ;
#10594 = CARTESIAN_POINT ( 'NONE',  ( 3.391751934957232706, -3.060691311048527652, 48.86415051386519082 ) ) ;
#10595 = CARTESIAN_POINT ( 'NONE',  ( 3.535533905932738197, -27.87500000000000000, -3.535533905932738197 ) ) ;
#10596 = CARTESIAN_POINT ( 'NONE',  ( 4.795541693661363958, 1.415196051561583790, 1.999999999999998224 ) ) ;
#10597 = FACE_OUTER_BOUND ( 'NONE', #12953, .T. ) ;
#10598 = CARTESIAN_POINT ( 'NONE',  ( 45.58845726811992449, 88.59290746114278647, -42.96152422706630603 ) ) ;
#10599 = CARTESIAN_POINT ( 'NONE',  ( 5.000000000000000000, -22.18750000273118772, 2.071067811865478614 ) ) ;
#10600 = ORIENTED_EDGE ( 'NONE', *, *, #867, .T. ) ;
#10601 = CARTESIAN_POINT ( 'NONE',  ( -4.458734124999999437, -22.00000000136559208, -1.846868145590735644 ) ) ;
#10602 = CARTESIAN_POINT ( 'NONE',  ( 6.439685834476867932, -4.942299687812352182, -7.659344964962495617 ) ) ;
#10603 = ORIENTED_EDGE ( 'NONE', *, *, #15712, .F. ) ;
#10604 = ORIENTED_EDGE ( 'NONE', *, *, #1623, .F. ) ;
#10605 = CARTESIAN_POINT ( 'NONE',  ( -5.000000000000000888, 6.123233995736767268E-16, -25.03750572909317285 ) ) ;
#10606 = LINE ( 'NONE', #9459, #677 ) ;
#10607 = ORIENTED_EDGE ( 'NONE', *, *, #2414, .F. ) ;
#10608 = ADVANCED_FACE ( 'NONE', ( #9722 ), #2291, .F. ) ;
#10609 = PLANE ( 'NONE',  #14266 ) ;
#10610 = CARTESIAN_POINT ( 'NONE',  ( 4.458734124999999437, -28.75000000136559208, 1.846868145590737864 ) ) ;
#10611 = DIRECTION ( 'NONE',  ( 0.000000000000000000, 1.000000000000000000, 0.000000000000000000 ) ) ;
#10612 = CYLINDRICAL_SURFACE ( 'NONE', #976, 2.649999999999992806 ) ;
#10613 = DIRECTION ( 'NONE',  ( -1.000000000000000000, 0.000000000000000000, 0.000000000000000000 ) ) ;
#10614 = CARTESIAN_POINT ( 'NONE',  ( -91.33974596215560382, -110.0591436588189396, 7.500000000000001776 ) ) ;
#10615 = CARTESIAN_POINT ( 'NONE',  ( 3.753672977998667726, 3.033343224707664376, -0.4999999986344072500 ) ) ;
#10616 = VERTEX_POINT ( 'NONE', #4881 ) ;
#10617 = ORIENTED_EDGE ( 'NONE', *, *, #6647, .T. ) ;
#10618 = CARTESIAN_POINT ( 'NONE',  ( -1.249327701956659542, 8.410337540185347294, -7.776713651266385696 ) ) ;
#10619 = VERTEX_POINT ( 'NONE', #14737 ) ;
#10620 = DIRECTION ( 'NONE',  ( 0.000000000000000000, 0.000000000000000000, -1.000000000000000000 ) ) ;
#10621 = CARTESIAN_POINT ( 'NONE',  ( 39.53738644056090124, -5.000000000000000000, 28.48076211354432985 ) ) ;
#10622 = CARTESIAN_POINT ( 'NONE',  ( -9.184850993605147944E-16, -28.25000000000000000, 5.000000000000000000 ) ) ;
#10623 = B_SPLINE_CURVE_WITH_KNOTS ( 'NONE', 3,
 ( #7974, #12877, #1812, #9102, #14103, #11356 ),
 .UNSPECIFIED., .F., .F.,
 ( 4, 2, 4 ),
 ( 0.004444412883774352327, 0.006655097293744444142, 0.008865781703714535958 ),
 .UNSPECIFIED. ) ;
#10624 = CARTESIAN_POINT ( 'NONE',  ( 5.381735091635035495, -0.5711823568785978633, -7.937499997268813168 ) ) ;
#10625 = CARTESIAN_POINT ( 'NONE',  ( -44.99999999999999289, -11.00000000000000178, -3.999999999999170885 ) ) ;
#10626 = CARTESIAN_POINT ( 'NONE',  ( 2.602085213965210642E-15, 8.660254037844392627, -9.999999999999998224 ) ) ;
#10627 = ORIENTED_EDGE ( 'NONE', *, *, #11721, .T. ) ;
#10628 = CARTESIAN_POINT ( 'NONE',  ( 7.500000000000000888, 4.330127018922199866, -1.000000000000000888 ) ) ;
#10629 = CARTESIAN_POINT ( 'NONE',  ( 2.602085213965210642E-15, 8.660254037844392627, -9.999999999999998224 ) ) ;
#10630 = CARTESIAN_POINT ( 'NONE',  ( 5.000000000000000000, -21.12500000273118772, 0.000000000000000000 ) ) ;
#10631 = ADVANCED_FACE ( 'NONE', ( #8683 ), #6257, .T. ) ;
#10632 = EDGE_LOOP ( 'NONE', ( #6303, #9725, #8472, #4555 ) ) ;
#10633 = CARTESIAN_POINT ( 'NONE',  ( 3.535533905932738197, -26.87500000000000000, -3.535533905932738197 ) ) ;
#10634 = ORIENTED_EDGE ( 'NONE', *, *, #13397, .F. ) ;
#10635 = ORIENTED_EDGE ( 'NONE', *, *, #4461, .T. ) ;
#10636 = CARTESIAN_POINT ( 'NONE',  ( 3.916244202832140253, -2.131511515620588160, -0.6874999986344089153 ) ) ;
#10637 = FACE_OUTER_BOUND ( 'NONE', #11659, .T. ) ;
#10638 = AXIS2_PLACEMENT_3D ( 'NONE', #9815, #14744, #8615 ) ;
#10639 = CARTESIAN_POINT ( 'NONE',  ( 3.061616997868383141E-16, -22.87500000273118772, -5.000000000000000000 ) ) ;
#10640 = CARTESIAN_POINT ( 'NONE',  ( -2.390265326283148806, -4.391654775818394363, -5.375000000000000888 ) ) ;
#10641 = DIRECTION ( 'NONE',  ( 1.000000000000000000, 0.000000000000000000, 1.114413700119375779E-16 ) ) ;
#10642 = CARTESIAN_POINT ( 'NONE',  ( 4.446142487674360488, -0.3868705316447643150, -0.3789984458506777676 ) ) ;
#10643 = DIRECTION ( 'NONE',  ( 0.000000000000000000, 1.000000000000000000, -0.000000000000000000 ) ) ;
#10644 = CARTESIAN_POINT ( 'NONE',  ( -6.762176242291807225E-13, 37.00000000000000000, 70.14999999999930935 ) ) ;
#10645 = DIRECTION ( 'NONE',  ( -0.000000000000000000, -1.000000000000000000, -0.000000000000000000 ) ) ;
#10646 = CARTESIAN_POINT ( 'NONE',  ( -3.916244202832140253, 2.131511515620587272, -1.937499998634406584 ) ) ;
#10647 = EDGE_LOOP ( 'NONE', ( #13730, #15484, #9099, #7492, #6569 ) ) ;
#10648 = CARTESIAN_POINT ( 'NONE',  ( 7.777900015783946408, 4.169681370001526943, -7.928862157988302073 ) ) ;
#10649 = EDGE_CURVE ( 'NONE', #13587, #10806, #2601, .T. ) ;
#10650 = ORIENTED_EDGE ( 'NONE', *, *, #8376, .F. ) ;
#10651 = ORIENTED_EDGE ( 'NONE', *, *, #1574, .F. ) ;
#10652 = ADVANCED_FACE ( 'NONE', ( #14904 ), #12328, .F. ) ;
#10653 = FILL_AREA_STYLE_COLOUR ( '', #894 ) ;
#10654 = CARTESIAN_POINT ( 'NONE',  ( -4.458734125000001214, -26.12500000136559919, 1.846868145590734089 ) ) ;
#10655 = DIRECTION ( 'NONE',  ( -0.000000000000000000, 1.000000000000000000, -0.000000000000000000 ) ) ;
#10656 = LINE ( 'NONE', #10417, #10225 ) ;
#10657 = CARTESIAN_POINT ( 'NONE',  ( -1.261996585732579224, 4.276409079477648589, -5.062499998634406140 ) ) ;
#10658 = DIRECTION ( 'NONE',  ( -0.000000000000000000, -1.000000000000000000, -0.000000000000000000 ) ) ;
#10659 = CARTESIAN_POINT ( 'NONE',  ( -5.000000000000000888, -27.43750000000000711, 2.071067811865474617 ) ) ;
#10660 = CARTESIAN_POINT ( 'NONE',  ( 0.5093500532425063732, 4.799145180956616130, -8.124999998634409692 ) ) ;
#10661 = CARTESIAN_POINT ( 'NONE',  ( -124.9999999999999858, -115.2072594216369907, 17.50000000000000000 ) ) ;
#10662 = FACE_OUTER_BOUND ( 'NONE', #13652, .T. ) ;
#10663 = CARTESIAN_POINT ( 'NONE',  ( 3.061616997868383141E-16, -21.87500000273118772, -5.000000000000000000 ) ) ;
#10664 = ORIENTED_EDGE ( 'NONE', *, *, #5683, .F. ) ;
#10665 = CARTESIAN_POINT ( 'NONE',  ( -4.458734125000000326, -22.87500000136559564, 1.846868145590734089 ) ) ;
#10666 = ADVANCED_FACE ( 'NONE', ( #202 ), #15958, .F. ) ;
#10667 = DIRECTION ( 'NONE',  ( 0.000000000000000000, 0.000000000000000000, 1.000000000000000000 ) ) ;
#10668 = EDGE_LOOP ( 'NONE', ( #4379, #2312, #13206, #12132 ) ) ;
#10669 = EDGE_LOOP ( 'NONE', ( #7470, #4074, #487, #7661, #13979, #181 ) ) ;
#10670 = EDGE_CURVE ( 'NONE', #7200, #4793, #13495, .T. ) ;
#10671 = LINE ( 'NONE', #4202, #14943 ) ;
#10672 = VECTOR ( 'NONE', #2740, 1000.000000000000114 ) ;
#10673 = CARTESIAN_POINT ( 'NONE',  ( -1.846868145590734756, -28.12500000136559564, -4.458734125000000326 ) ) ;
#10674 = DIRECTION ( 'NONE',  ( -1.000000000000000000, 0.000000000000000000, 9.048317650695024227E-15 ) ) ;
#10675 = VERTEX_POINT ( 'NONE', #5122 ) ;
#10676 = DIRECTION ( 'NONE',  ( 1.000000000000000000, 0.000000000000000000, 0.000000000000000000 ) ) ;
#10677 = PRODUCT_DEFINITION_SHAPE ( 'NONE', 'NONE',  #501 ) ;
#10678 = CIRCLE ( 'NONE', #13745, 5.000000000000000000 ) ;
#10679 = LINE ( 'NONE', #10757, #9117 ) ;
#10680 = CARTESIAN_POINT ( 'NONE',  ( -1.846868145590737420, -29.00000000136559564, 4.458734124999999437 ) ) ;
#10681 = CARTESIAN_POINT ( 'NONE',  ( 4.175002511812151873, 2.208363329454889445, -3.469254087858244073 ) ) ;
#10682 = LINE ( 'NONE', #13005, #10816 ) ;
#10683 = DIRECTION ( 'NONE',  ( 3.343241100358131282E-16, 0.000000000000000000, -1.000000000000000000 ) ) ;
#10684 = DIRECTION ( 'NONE',  ( 0.000000000000000000, 0.000000000000000000, 1.000000000000000000 ) ) ;
#10685 = VERTEX_POINT ( 'NONE', #12293 ) ;
#10686 = EDGE_CURVE ( 'NONE', #12917, #1672, #3277, .T. ) ;
#10687 = EDGE_LOOP ( 'NONE', ( #15836, #10727, #15366, #4941 ) ) ;
#10688 = CARTESIAN_POINT ( 'NONE',  ( -4.000000000000000888, 1.563622288139195238, -0.2253451193528307472 ) ) ;
#10689 = ORIENTED_EDGE ( 'NONE', *, *, #713, .T. ) ;
#10690 = PRESENTATION_LAYER_ASSIGNMENT (  '', '', ( #14306 ) ) ;
#10691 = CARTESIAN_POINT ( 'NONE',  ( -5.725490332117410652, 0.000000000000000000, 49.91684015347181003 ) ) ;
#10692 =( BOUNDED_CURVE ( )  B_SPLINE_CURVE ( 2, ( #62, #9662, #3521, #3683, #6039, #7417, #13289, #13376, #9590 ),
 .UNSPECIFIED., .F., .F. ) 
 B_SPLINE_CURVE_WITH_KNOTS ( ( 3, 2, 2, 2, 3 ),
 ( 0.07500000000000006661, 0.08750000000000007772, 0.1000000000000000888, 0.1125000000000000999, 0.1250000000000001110 ),
 .UNSPECIFIED. ) 
 CURVE ( )  GEOMETRIC_REPRESENTATION_ITEM ( )  RATIONAL_B_SPLINE_CURVE ( ( 0.9999999999999995559, 0.9238795325112871826, 1.000000000000000000, 0.9238795325112867385, 1.000000000000000000, 0.9238795325112867385, 1.000000000000000000, 0.9238795325112860723, 1.000000000000000666 ) ) 
 REPRESENTATION_ITEM ( '' )  );
#10693 = CIRCLE ( 'NONE', #8909, 2.500000000000000444 ) ;
#10694 = CARTESIAN_POINT ( 'NONE',  ( 11.91154273188008439, 0.000000000000000000, 56.63139720814412925 ) ) ;
#10695 = CARTESIAN_POINT ( 'NONE',  ( -3.916244202832140253, 2.131511515620587272, 1.062500001365592528 ) ) ;
#10696 = DIRECTION ( 'NONE',  ( 0.000000000000000000, -1.000000000000000000, 0.000000000000000000 ) ) ;
#10697 = CARTESIAN_POINT ( 'NONE',  ( 1.261996585732578113, -4.276409079477644148, -2.812499998634407472 ) ) ;
#10698 = CARTESIAN_POINT ( 'NONE',  ( -4.391654775818395251, 2.390265326283148806, -0.6250000000000005551 ) ) ;
#10699 = LINE ( 'NONE', #9488, #13890 ) ;
#10700 = EDGE_LOOP ( 'NONE', ( #4463, #2788, #8471, #9123 ) ) ;
#10701 = DIRECTION ( 'NONE',  ( 0.5000000000000004441, -0.8660254037844383745, 0.000000000000000000 ) ) ;
#10702 = CARTESIAN_POINT ( 'NONE',  ( 5.000000000000004441, -2.247904837838113790E-16, -2.920263044861759472 ) ) ;
#10703 = EDGE_CURVE ( 'NONE', #15838, #7550, #6458, .T. ) ;
#10704 = FACE_OUTER_BOUND ( 'NONE', #9824, .T. ) ;
#10705 = VERTEX_POINT ( 'NONE', #3897 ) ;
#10706 = CARTESIAN_POINT ( 'NONE',  ( 0.000000000000000000, -13.00000000000000178, 1.500000000000000000 ) ) ;
#10707 = ORIENTED_EDGE ( 'NONE', *, *, #6935, .T. ) ;
#10708 = AXIS2_PLACEMENT_3D ( 'NONE', #13697, #384, #4087 ) ;
#10709 = EDGE_LOOP ( 'NONE', ( #6574, #4102 ) ) ;
#10710 = CARTESIAN_POINT ( 'NONE',  ( 0.5789871446316211534, 4.420982230657665824, -0.3789984458506777676 ) ) ;
#10711 = DIRECTION ( 'NONE',  ( 0.4999999999999998335, -0.000000000000000000, 0.8660254037844387076 ) ) ;
#10712 = CARTESIAN_POINT ( 'NONE',  ( 4.000000000000000888, 1.539600717838996990, -3.300726591567079815 ) ) ;
#10713 = MECHANICAL_DESIGN_GEOMETRIC_PRESENTATION_REPRESENTATION (  '', ( #7882 ), #911 ) ;
#10714 = AXIS2_PLACEMENT_3D ( 'NONE', #14646, #15628, #6985 ) ;
#10715 = EDGE_CURVE ( 'NONE', #9186, #12918, #5669, .T. ) ;
#10716 = LINE ( 'NONE', #2134, #3012 ) ;
#10717 = CARTESIAN_POINT ( 'NONE',  ( 0.000000000000000000, 40.00000000000000000, 0.000000000000000000 ) ) ;
#10718 = AXIS2_PLACEMENT_3D ( 'NONE', #13590, #11176, #118 ) ;
#10719 = FACE_OUTER_BOUND ( 'NONE', #8929, .T. ) ;
#10720 = CARTESIAN_POINT ( 'NONE',  ( -4.795541693661363958, -1.415196051561583790, -7.500000000000003553 ) ) ;
#10721 = DIRECTION ( 'NONE',  ( -0.8660254037844408170, 0.000000000000000000, -0.4999999999999961142 ) ) ;
#10722 = CARTESIAN_POINT ( 'NONE',  ( 3.152801135295367541, -30.56250000136559564, -3.152801135295367541 ) ) ;
#10723 = CARTESIAN_POINT ( 'NONE',  ( -4.799145180956616130, 0.5093500532425063732, 1.125000001365592306 ) ) ;
#10724 = EDGE_LOOP ( 'NONE', ( #4578, #543, #11682, #4516 ) ) ;
#10725 = DIRECTION ( 'NONE',  ( -1.000000000000000000, 0.000000000000000000, 0.000000000000000000 ) ) ;
#10726 = ORIENTED_EDGE ( 'NONE', *, *, #1072, .F. ) ;
#10727 = ORIENTED_EDGE ( 'NONE', *, *, #14729, .F. ) ;
#10728 = VERTEX_POINT ( 'NONE', #15228 ) ;
#10729 = CARTESIAN_POINT ( 'NONE',  ( 2.730187237215162345E-16, -27.43750000136559564, -4.458734124999999437 ) ) ;
#10730 = CARTESIAN_POINT ( 'NONE',  ( 2.500000000000000888, 3.061616997868384127E-16, -4.974599999999998801 ) ) ;
#10731 = CARTESIAN_POINT ( 'NONE',  ( -124.9999999999999716, -115.2072594216369623, -13.35786437626904721 ) ) ;
#10732 = EDGE_CURVE ( 'NONE', #10466, #15821, #7957, .T. ) ;
#10733 = EDGE_CURVE ( 'NONE', #7722, #6759, #14970, .T. ) ;
#10734 = CARTESIAN_POINT ( 'NONE',  ( -3.753672977998669502, -3.033343224707661712, -4.749999998634407028 ) ) ;
#10735 = CARTESIAN_POINT ( 'NONE',  ( -3.974344831685191280E-13, 4.796734841935104576, -3.721909803043223608 ) ) ;
#10736 = ADVANCED_FACE ( 'NONE', ( #14081 ), #12533, .F. ) ;
#10737 = CARTESIAN_POINT ( 'NONE',  ( -2.071067811865475061, -22.68749999999999645, -5.000000000000000888 ) ) ;
#10738 = AXIS2_PLACEMENT_3D ( 'NONE', #13367, #9359, #10725 ) ;
#10739 = CARTESIAN_POINT ( 'NONE',  ( 1.415196051561583790, -4.795541693661363958, 0.7499999999999972244 ) ) ;
#10740 = CARTESIAN_POINT ( 'NONE',  ( -5.000000000000000888, -21.68750000273119127, -2.071067811865475949 ) ) ;
#10741 = CARTESIAN_POINT ( 'NONE',  ( 0.000000000000000000, 0.000000000000000000, 0.000000000000000000 ) ) ;
#10742 = CARTESIAN_POINT ( 'NONE',  ( -4.458734124999999437, -28.93750000136559564, -5.460374474430324690E-16 ) ) ;
#10743 = CIRCLE ( 'NONE', #7395, 5.000000000000000000 ) ;
#10744 = EDGE_LOOP ( 'NONE', ( #5920, #4259, #115, #14639 ) ) ;
#10745 = CARTESIAN_POINT ( 'NONE',  ( -1.846868145590737420, -21.75000000136559208, 4.458734124999997661 ) ) ;
#10746 = DIRECTION ( 'NONE',  ( 0.8660254037844384856, 0.000000000000000000, 0.5000000000000004441 ) ) ;
#10747 = VERTEX_POINT ( 'NONE', #6571 ) ;
#10748 = VERTEX_POINT ( 'NONE', #2679 ) ;
#10749 = LINE ( 'NONE', #14465, #1786 ) ;
#10750 = CARTESIAN_POINT ( 'NONE',  ( -4.458734125000000326, -29.00000000136559564, -1.846868145590735644 ) ) ;
#10751 = CARTESIAN_POINT ( 'NONE',  ( -5.000000000000000888, 6.123233995736767268E-16, -25.03750572909317285 ) ) ;
#10752 = EDGE_LOOP ( 'NONE', ( #2015, #14617, #93, #10825, #12231, #8866, #6318, #1993 ) ) ;
#10753 = DIRECTION ( 'NONE',  ( 0.000000000000000000, 1.000000000000000000, 0.000000000000000000 ) ) ;
#10754 = CIRCLE ( 'NONE', #13565, 4.000000000000000000 ) ;
#10755 = AXIS2_PLACEMENT_3D ( 'NONE', #2435, #7388, #12295 ) ;
#10756 = CARTESIAN_POINT ( 'NONE',  ( 7.102951435054648059E-15, 2.000000000000001776, 57.99999999999999289 ) ) ;
#10757 = CARTESIAN_POINT ( 'NONE',  ( -2.059999999999998721, 2.522772406243545965E-16, -0.3080913168122742518 ) ) ;
#10758 = EDGE_CURVE ( 'NONE', #14589, #13263, #12770, .T. ) ;
#10759 = PRODUCT_RELATED_PRODUCT_CATEGORY ( 'part', '', ( #6036 ) ) ;
#10760 = CARTESIAN_POINT ( 'NONE',  ( 3.152801135295367541, -29.56250000136559208, -3.152801135295367541 ) ) ;
#10761 = CARTESIAN_POINT ( 'NONE',  ( -28.86751345948126612, -35.00000000000000000, -18.00000000000000355 ) ) ;
#10762 = VECTOR ( 'NONE', #13865, 1000.000000000000000 ) ;
#10763 = DIRECTION ( 'NONE',  ( 0.4999999999999998890, 0.000000000000000000, 0.8660254037844388186 ) ) ;
#10764 = DIRECTION ( 'NONE',  ( 0.000000000000000000, 1.000000000000000000, 0.000000000000000000 ) ) ;
#10765 = ORIENTED_EDGE ( 'NONE', *, *, #6255, .T. ) ;
#10766 = CIRCLE ( 'NONE', #958, 3.499999999999999556 ) ;
#10767 =( NAMED_UNIT ( * ) PLANE_ANGLE_UNIT ( ) SI_UNIT ( $, .RADIAN. ) );
#10768 = ORIENTED_EDGE ( 'NONE', *, *, #7153, .F. ) ;
#10769 = CARTESIAN_POINT ( 'NONE',  ( -2.325424218458715053, 7.317669739337203438, -7.030005583190798824 ) ) ;
#10770 = ORIENTED_EDGE ( 'NONE', *, *, #6546, .T. ) ;
#10771 = B_SPLINE_CURVE_WITH_KNOTS ( 'NONE', 3,
 ( #9490, #11588, #14101, #13029 ),
 .UNSPECIFIED., .F., .F.,
 ( 4, 4 ),
 ( 0.001452767664617488205, 0.002080905508140416978 ),
 .UNSPECIFIED. ) ;
#10772 = VECTOR ( 'NONE', #8125, 1000.000000000000000 ) ;
#10773 = PLANE ( 'NONE',  #6583 ) ;
#10774 = EDGE_CURVE ( 'NONE', #2789, #10280, #6745, .T. ) ;
#10775 = ADVANCED_FACE ( 'NONE', ( #10130 ), #10215, .F. ) ;
#10776 = DIRECTION ( 'NONE',  ( 1.224646799147353207E-16, 1.000000000000000000, -0.000000000000000000 ) ) ;
#10777 = CARTESIAN_POINT ( 'NONE',  ( -3.753672977998669946, -3.033343224707661712, -0.7499999986344074721 ) ) ;
#10778 = DIRECTION ( 'NONE',  ( 6.123233995736766036E-17, 1.000000000000000000, 0.000000000000000000 ) ) ;
#10779 = CARTESIAN_POINT ( 'NONE',  ( -1.261996585732579224, 4.276409079477648589, -1.312499998634406140 ) ) ;
#10780 = CIRCLE ( 'NONE', #14178, 9.999999999999994671 ) ;
#10781 = CARTESIAN_POINT ( 'NONE',  ( -60.00000000000000000, -35.00000000000000000, 17.99999999999999289 ) ) ;
#10782 = VERTEX_POINT ( 'NONE', #360 ) ;
#10783 = LINE ( 'NONE', #10855, #14164 ) ;
#10784 = CARTESIAN_POINT ( 'NONE',  ( 1.567478505476134606E-15, 4.618802153517012066, -5.000000000000000000 ) ) ;
#10785 = ORIENTED_EDGE ( 'NONE', *, *, #4507, .F. ) ;
#10786 = CYLINDRICAL_SURFACE ( 'NONE', #6187, 3.499999999999999556 ) ;
#10787 = ORIENTED_EDGE ( 'NONE', *, *, #7555, .F. ) ;
#10788 = AXIS2_PLACEMENT_3D ( 'NONE', #4154, #132, #2617 ) ;
#10789 = ORIENTED_EDGE ( 'NONE', *, *, #11885, .F. ) ;
#10790 = CARTESIAN_POINT ( 'NONE',  ( 3.061616997868383141E-16, -30.75000000000000000, -5.000000000000000000 ) ) ;
#10791 =( BOUNDED_SURFACE ( )  B_SPLINE_SURFACE ( 3, 2, ( 
 ( #13703, #2715, #12409 ),
 ( #9912, #15178, #4008 ),
 ( #5310, #1666, #4095 ),
 ( #8960, #6608, #9045 ),
 ( #10090, #390, #13948 ),
 ( #12651, #14941, #1426 ) ),
 .UNSPECIFIED., .F., .F., .F. ) 
 B_SPLINE_SURFACE_WITH_KNOTS ( ( 4, 2, 4 ),
 ( 3, 3 ),
 ( 0.02032853247518126918, 0.02278863295364821906, 0.02524873343211516893 ),
 ( 0.000000000000000000, 1.000000000000000000 ),
 .UNSPECIFIED. ) 
 GEOMETRIC_REPRESENTATION_ITEM ( )  RATIONAL_B_SPLINE_SURFACE ( (
 ( 1.000000000000000000, 0.8047781615896838492, 1.000000000000000000),
 ( 1.000000000000000000, 0.8123767586288186404, 1.000000000000000000),
 ( 1.000000000000000000, 0.8190662415565814758, 1.000000000000000000),
 ( 1.000000000000000000, 0.8192361015667604107, 1.000000000000000000),
 ( 1.000000000000000000, 0.8126135807104967190, 1.000000000000000000),
 ( 1.000000000000000000, 0.8047712338318580017, 1.000000000000000000) ) ) 
 REPRESENTATION_ITEM ( '' )  SURFACE ( )  );
#10792 = DIRECTION ( 'NONE',  ( 0.000000000000000000, 0.000000000000000000, -1.000000000000000000 ) ) ;
#10793 = AXIS2_PLACEMENT_3D ( 'NONE', #11989, #8385, #3363 ) ;
#10794 = AXIS2_PLACEMENT_3D ( 'NONE', #11645, #1715, #7799 ) ;
#10795 = ADVANCED_FACE ( 'NONE', ( #5443 ), #1477, .T. ) ;
#10796 = CYLINDRICAL_SURFACE ( 'NONE', #5604, 25.00000000000000000 ) ;
#10797 = CARTESIAN_POINT ( 'NONE',  ( 41.26943724812357317, -3.000000000000000000, -27.48076211352550047 ) ) ;
#10798 = CARTESIAN_POINT ( 'NONE',  ( 11.91154273188008084, -5.000000000000000000, 56.63139720814412925 ) ) ;
#10799 = VECTOR ( 'NONE', #6388, 1000.000000000000000 ) ;
#10800 = CYLINDRICAL_SURFACE ( 'NONE', #4584, 5.000000000000000888 ) ;
#10801 = DIRECTION ( 'NONE',  ( -0.000000000000000000, -1.000000000000000000, -0.000000000000000000 ) ) ;
#10802 = CARTESIAN_POINT ( 'NONE',  ( -3.152801135295367985, -30.06250000136559564, 3.152801135295367096 ) ) ;
#10803 = CARTESIAN_POINT ( 'NONE',  ( 4.276409079477644148, 1.261996585732577891, 1.687500001365593194 ) ) ;
#10804 = ORIENTED_EDGE ( 'NONE', *, *, #8327, .F. ) ;
#10805 = CARTESIAN_POINT ( 'NONE',  ( -0.3483149870578519658, 8.861353789385018942, -7.493854785173811983 ) ) ;
#10806 = VERTEX_POINT ( 'NONE', #11410 ) ;
#10807 = AXIS2_PLACEMENT_3D ( 'NONE', #3669, #6739, #12462 ) ;
#10808 = ORIENTED_EDGE ( 'NONE', *, *, #2042, .F. ) ;
#10809 = AXIS2_PLACEMENT_3D ( 'NONE', #15155, #7739, #13851 ) ;
#10810 = ORIENTED_EDGE ( 'NONE', *, *, #14209, .F. ) ;
#10811 = CARTESIAN_POINT ( 'NONE',  ( -4.458734124999999437, -26.18750000136559919, -5.460374474430324690E-16 ) ) ;
#10812 = CYLINDRICAL_SURFACE ( 'NONE', #3500, 2.649999999999992806 ) ;
#10813 = AXIS2_PLACEMENT_3D ( 'NONE', #5999, #7374, #6169 ) ;
#10814 = FACE_OUTER_BOUND ( 'NONE', #7784, .T. ) ;
#10815 = DIRECTION ( 'NONE',  ( 1.000000000000000000, 0.000000000000000000, 0.000000000000000000 ) ) ;
#10816 = VECTOR ( 'NONE', #668, 999.9999999999998863 ) ;
#10817 = CIRCLE ( 'NONE', #14681, 1.999999999999998224 ) ;
#10818 = FACE_OUTER_BOUND ( 'NONE', #12017, .T. ) ;
#10819 = CARTESIAN_POINT ( 'NONE',  ( -4.795541693661363958, -1.415196051561583790, -2.500000000000002220 ) ) ;
#10820 = LINE ( 'NONE', #9595, #12738 ) ;
#10821 = CARTESIAN_POINT ( 'NONE',  ( -0.03800824613358327192, -4.872903691120612280, -0.09399265280457684557 ) ) ;
#10822 = CARTESIAN_POINT ( 'NONE',  ( -3.535533905932737309, -21.75000000273118772, -3.535533905932738197 ) ) ;
#10823 = EDGE_LOOP ( 'NONE', ( #11805, #9178 ) ) ;
#10824 = PLANE ( 'NONE',  #14332 ) ;
#10825 = ORIENTED_EDGE ( 'NONE', *, *, #601, .T. ) ;
#10826 = EDGE_LOOP ( 'NONE', ( #2362, #6479, #14191, #11157, #13658 ) ) ;
#10827 = CARTESIAN_POINT ( 'NONE',  ( 3.152801135295366208, -29.56250000136559208, 3.152801135295367985 ) ) ;
#10828 = ADVANCED_FACE ( 'NONE', ( #2765 ), #4139, .T. ) ;
#10829 = DIRECTION ( 'NONE',  ( 0.000000000000000000, 1.000000000000000000, 0.000000000000000000 ) ) ;
#10830 = ORIENTED_EDGE ( 'NONE', *, *, #10845, .F. ) ;
#10832 = AXIS2_PLACEMENT_3D ( 'NONE', #10706, #15801, #12057 ) ;
#10831 = CARTESIAN_POINT ( 'NONE',  ( -67.50000000000000000, 37.00000000000000000, 2.649999999999278710 ) ) ;
#10833 = DIRECTION ( 'NONE',  ( -0.000000000000000000, -0.000000000000000000, -1.000000000000000000 ) ) ;
#10834 = CARTESIAN_POINT ( 'NONE',  ( 19.99999999999956657, -8.786575603324269439E-13, 1.500000000000000000 ) ) ;
#10835 = CARTESIAN_POINT ( 'NONE',  ( -91.33974596215560382, -110.0591436588189396, 17.50000000000000000 ) ) ;
#10836 = CARTESIAN_POINT ( 'NONE',  ( -4.458734125000000326, -23.25000000136559208, -1.846868145590735644 ) ) ;
#10837 = DIRECTION ( 'NONE',  ( -1.000000000000000000, -0.000000000000000000, -0.000000000000000000 ) ) ;
#10838 = CARTESIAN_POINT ( 'NONE',  ( -3.264650091097280831E-13, -4.796980096169642493, -3.721999068284424617 ) ) ;
#10839 = CARTESIAN_POINT ( 'NONE',  ( -5.000000000000004441, -1.011557177027151181E-15, -5.545263047592944972 ) ) ;
#10840 = CARTESIAN_POINT ( 'NONE',  ( 10.00000000000098765, -13.00000000000000178, 17.32050807568871065 ) ) ;
#10841 = ORIENTED_EDGE ( 'NONE', *, *, #9791, .F. ) ;
#10843 = ORIENTED_EDGE ( 'NONE', *, *, #9852, .F. ) ;
#10842 = EDGE_CURVE ( 'NONE', #11920, #4817, #12618, .T. ) ;
#10844 = DIRECTION ( 'NONE',  ( 0.000000000000000000, 1.000000000000000000, 0.000000000000000000 ) ) ;
#10845 = EDGE_CURVE ( 'NONE', #5764, #7493, #15757, .T. ) ;
#10846 = ORIENTED_EDGE ( 'NONE', *, *, #7861, .T. ) ;
#10847 = CARTESIAN_POINT ( 'NONE',  ( 5.200000000000002842, 3.306546357697854226E-16, 2.700000000000000622 ) ) ;
#10848 = CARTESIAN_POINT ( 'NONE',  ( -9.184850993605147944E-16, -25.37500000273118417, 5.000000000000000000 ) ) ;
#10849 = CARTESIAN_POINT ( 'NONE',  ( 4.799145180956616130, -0.5093500532425063732, -1.374999998634406140 ) ) ;
#10850 = DIRECTION ( 'NONE',  ( 0.000000000000000000, 0.000000000000000000, 1.000000000000000000 ) ) ;
#10851 = CARTESIAN_POINT ( 'NONE',  ( 0.5093500532425063732, 4.799145180956616130, -0.3749999986344090264 ) ) ;
#10852 = CARTESIAN_POINT ( 'NONE',  ( -90.00000000000000000, -35.00000000000000711, 17.50000000000000000 ) ) ;
#10853 = DIRECTION ( 'NONE',  ( 0.8660254037844384856, 0.000000000000000000, 0.5000000000000001110 ) ) ;
#10854 = ORIENTED_EDGE ( 'NONE', *, *, #3445, .T. ) ;
#10855 = CARTESIAN_POINT ( 'NONE',  ( -44.45597072760116220, -35.00000000000000000, -41.00000000000001421 ) ) ;
#10856 = EDGE_CURVE ( 'NONE', #5667, #1764, #12691, .T. ) ;
#10857 = EDGE_LOOP ( 'NONE', ( #267, #5933 ) ) ;
#10858 = CARTESIAN_POINT ( 'NONE',  ( -114.9999999999999716, -10.00000000000000888, 7.500000000000001776 ) ) ;
#10859 = EDGE_LOOP ( 'NONE', ( #10804, #8262, #13158, #2073, #9966, #14230, #12597, #229 ) ) ;
#10860 = ORIENTED_EDGE ( 'NONE', *, *, #9310, .T. ) ;
#10861 = EDGE_CURVE ( 'NONE', #4061, #15286, #435, .T. ) ;
#10862 = ORIENTED_EDGE ( 'NONE', *, *, #9598, .F. ) ;
#10863 = CARTESIAN_POINT ( 'NONE',  ( 3.753672977998667726, 3.033343224707664820, -1.499999998634408138 ) ) ;
#10864 = CARTESIAN_POINT ( 'NONE',  ( -35.00000000000000000, 40.00000000000000000, 0.000000000000000000 ) ) ;
#10865 = CARTESIAN_POINT ( 'NONE',  ( 7.500000000000000000, 4.330127018922190096, -9.999999999999998224 ) ) ;
#10866 = MECHANICAL_DESIGN_GEOMETRIC_PRESENTATION_REPRESENTATION (  '', ( #4922 ), #4702 ) ;
#10867 = DIRECTION ( 'NONE',  ( 1.000000000000000000, 0.000000000000000000, 0.000000000000000000 ) ) ;
#10868 = CARTESIAN_POINT ( 'NONE',  ( -4.391654775818395251, 2.390265326283148806, -0.4999999972688171090 ) ) ;
#10869 = CARTESIAN_POINT ( 'NONE',  ( 10.17949192431120586, -5.000000000000000000, 57.63139720814412215 ) ) ;
#10870 = SURFACE_STYLE_USAGE ( .BOTH. , #1087 ) ;
#10871 = CARTESIAN_POINT ( 'NONE',  ( 3.152801135295367541, -27.56250000136559564, -3.152801135295367541 ) ) ;
#10872 = CARTESIAN_POINT ( 'NONE',  ( -3.033343224707664376, 3.753672977998667726, -4.999999998634407028 ) ) ;
#10873 = ORIENTED_EDGE ( 'NONE', *, *, #10252, .T. ) ;
#10874 = CARTESIAN_POINT ( 'NONE',  ( 1.013163106017221704, 8.075304045852348622, -7.231838333420562037 ) ) ;
#10875 = EDGE_CURVE ( 'NONE', #560, #15871, #9399, .T. ) ;
#10876 = VERTEX_POINT ( 'NONE', #8355 ) ;
#10877 = ORIENTED_EDGE ( 'NONE', *, *, #11555, .F. ) ;
#10878 =( BOUNDED_CURVE ( )  B_SPLINE_CURVE ( 2, ( #5352, #13981, #1549, #10290, #6487, #10438, #12760, #11401, #14070, #5264, #10203 ),
 .UNSPECIFIED., .F., .F. ) 
 B_SPLINE_CURVE_WITH_KNOTS ( ( 3, 2, 2, 2, 2, 3 ),
 ( 0.2545872658012772738, 0.2625000000000000111, 0.2750000000000000222, 0.2874999999999999778, 0.2999999999999999889, 0.3045872658012772627 ),
 .UNSPECIFIED. ) 
 CURVE ( )  GEOMETRIC_REPRESENTATION_ITEM ( )  RATIONAL_B_SPLINE_CURVE ( ( 0.9646335149384808183, 0.9518143178943437865, 1.000000000000000000, 0.9238795325112867385, 1.000000000000000000, 0.9238795325112867385, 1.000000000000000000, 0.9238795325112867385, 1.000000000000000000, 0.9720652146169430630, 0.9646335149384808183 ) ) 
 REPRESENTATION_ITEM ( '' )  );
#10879 = EDGE_CURVE ( 'NONE', #395, #7055, #6901, .T. ) ;
#10880 = EDGE_LOOP ( 'NONE', ( #8284, #13666, #12856, #11212 ) ) ;
#10881 = CARTESIAN_POINT ( 'NONE',  ( 3.152801135295367541, -22.56250000136559564, -3.152801135295367541 ) ) ;
#10882 = CARTESIAN_POINT ( 'NONE',  ( 0.000000000000000000, 0.000000000000000000, -0.2800830152838844622 ) ) ;
#10883 = CARTESIAN_POINT ( 'NONE',  ( -45.00000000000000000, 0.000000000000000000, 17.50000000000000000 ) ) ;
#10884 = DIRECTION ( 'NONE',  ( -0.000000000000000000, 1.000000000000000000, -0.000000000000000000 ) ) ;
#10885 = CARTESIAN_POINT ( 'NONE',  ( -114.9999999999999858, -109.4337567297407219, 17.50000000000000000 ) ) ;
#10886 = VECTOR ( 'NONE', #4047, 1000.000000000000000 ) ;
#10887 = CARTESIAN_POINT ( 'NONE',  ( 3.535533905932736864, -23.12500000000000000, 3.535533905932738641 ) ) ;
#10888 = CARTESIAN_POINT ( 'NONE',  ( -3.401574460001764777, 4.209348295687701302, -0.6875000000000016653 ) ) ;
#10889 = CARTESIAN_POINT ( 'NONE',  ( -5.000000000000004441, -1.011557177027151181E-15, -3.545263047592942307 ) ) ;
#10890 = DIRECTION ( 'NONE',  ( 0.000000000000000000, -1.000000000000000000, 0.000000000000000000 ) ) ;
#10891 = CARTESIAN_POINT ( 'NONE',  ( -3.535533905932738641, -21.50000000273118772, 3.535533905932737309 ) ) ;
#10892 = CARTESIAN_POINT ( 'NONE',  ( 2.131511515620586383, 3.916244202832140253, 0.5625000013655921949 ) ) ;
#10893 = VERTEX_POINT ( 'NONE', #14250 ) ;
#10894 = DIRECTION ( 'NONE',  ( -0.5000000000000003331, -2.168404344971013059E-16, 0.8660254037844384856 ) ) ;
#10895 = ORIENTED_EDGE ( 'NONE', *, *, #10686, .T. ) ;
#10896 = B_SPLINE_CURVE_WITH_KNOTS ( 'NONE', 3,
 ( #547, #5464, #12476, #1415, #309, #4083, #10327, #9036, #15252, #230 ),
 .UNSPECIFIED., .F., .F.,
 ( 4, 2, 2, 2, 4 ),
 ( 0.000000000000000000, 0.002305503304226492935, 0.004611006608452985871, 0.006916509912679479240, 0.009222013216905970007 ),
 .UNSPECIFIED. ) ;
#10897 = ORIENTED_EDGE ( 'NONE', *, *, #1043, .F. ) ;
#10898 = CARTESIAN_POINT ( 'NONE',  ( -7.500000000000003553, -4.732323933430408580, -7.493854309896105015 ) ) ;
#10899 = EDGE_CURVE ( 'NONE', #5290, #11376, #10012, .T. ) ;
#10900 = CARTESIAN_POINT ( 'NONE',  ( 1.846868145590735200, -27.25000000136559564, -4.458734125000000326 ) ) ;
#10901 = LINE ( 'NONE', #13393, #10242 ) ;
#10902 = ORIENTED_EDGE ( 'NONE', *, *, #6366, .T. ) ;
#10903 = CARTESIAN_POINT ( 'NONE',  ( 35.00000000000000000, 50.00000000000000000, 0.000000000000000000 ) ) ;
#10904 = CARTESIAN_POINT ( 'NONE',  ( 0.000000000000000000, 20.00000000000000000, 0.000000000000000000 ) ) ;
#10905 = DIRECTION ( 'NONE',  ( -0.000000000000000000, -1.000000000000000000, -0.000000000000000000 ) ) ;
#10906 = SHAPE_REPRESENTATION ( 'socket head cap screw_iso_ISO 4762 M5 x 12 - 12N', ( #3223 ), #7865 ) ;
#10907 = CARTESIAN_POINT ( 'NONE',  ( 4.174999999999999822, 0.000000000000000000, -0.5776712190230133270 ) ) ;
#10908 = CARTESIAN_POINT ( 'NONE',  ( -4.458734124999999437, -22.18750000136559564, -5.460374474430324690E-16 ) ) ;
#10909 = DIRECTION ( 'NONE',  ( -0.5000000000000051070, 0.000000000000000000, 0.8660254037844355990 ) ) ;
#10910 = EDGE_CURVE ( 'NONE', #8643, #6940, #11959, .T. ) ;
#10911 = CARTESIAN_POINT ( 'NONE',  ( 1.415196051561583790, -4.795541693661363958, -1.124999997268814278 ) ) ;
#10912 = FILL_AREA_STYLE ('',( #9393 ) ) ;
#10913 = CARTESIAN_POINT ( 'NONE',  ( 7.263825692932296185, 4.945657111639574666, -7.907570769506047981 ) ) ;
#10914 = VECTOR ( 'NONE', #3091, 1000.000000000000000 ) ;
#10915 = CARTESIAN_POINT ( 'NONE',  ( 0.000000000000000000, -13.00000000000000178, 0.000000000000000000 ) ) ;
#10916 = CARTESIAN_POINT ( 'NONE',  ( 3.535533905932736864, -25.12500000000000000, 3.535533905932738641 ) ) ;
#10917 = AXIS2_PLACEMENT_3D ( 'NONE', #1122, #6062, #15930 ) ;
#10918 = EDGE_LOOP ( 'NONE', ( #13031, #14644, #506, #1077, #4717 ) ) ;
#10919 = VERTEX_POINT ( 'NONE', #5834 ) ;
#10920 = LINE ( 'NONE', #8751, #6345 ) ;
#10921 = ORIENTED_EDGE ( 'NONE', *, *, #6341, .T. ) ;
#10922 = CARTESIAN_POINT ( 'NONE',  ( -2.071067811865492381, -26.31250000000000355, 4.999999999999985789 ) ) ;
#10923 = CARTESIAN_POINT ( 'NONE',  ( 0.000000000000000000, 5.051668046482832750E-16, -4.000000000000000000 ) ) ;
#10924 = EDGE_CURVE ( 'NONE', #8883, #13974, #2110, .T. ) ;
#10925 = CARTESIAN_POINT ( 'NONE',  ( -0.5093500532425060401, -4.799145180956616130, -1.624999998634406362 ) ) ;
#10926 = ADVANCED_FACE ( 'NONE', ( #910 ), #14708, .F. ) ;
#10927 = CARTESIAN_POINT ( 'NONE',  ( -21.01110699893042622, 6.999999999999999112, -36.39230484541335642 ) ) ;
#10928 = PRODUCT_DEFINITION_SHAPE ( 'NONE', 'NONE',  #11724 ) ;
#10930 = VECTOR ( 'NONE', #3286, 1000.000000000000000 ) ;
#10929 = CARTESIAN_POINT ( 'NONE',  ( 3.753672977998667726, 3.033343224707664376, -2.499999998634408804 ) ) ;
#10931 = FACE_OUTER_BOUND ( 'NONE', #10632, .T. ) ;
#10932 =( NAMED_UNIT ( * ) SI_UNIT ( $, .STERADIAN. ) SOLID_ANGLE_UNIT ( ) );
#10933 = ORIENTED_EDGE ( 'NONE', *, *, #2261, .F. ) ;
#10934 = DIRECTION ( 'NONE',  ( 0.000000000000000000, 0.000000000000000000, -1.000000000000000000 ) ) ;
#10935 = VERTEX_POINT ( 'NONE', #3101 ) ;
#10936 = CARTESIAN_POINT ( 'NONE',  ( 4.000000000000000000, -1.677850389431204459, -3.535268758346977513 ) ) ;
#10937 = ORIENTED_EDGE ( 'NONE', *, *, #2152, .F. ) ;
#10938 =( GEOMETRIC_REPRESENTATION_CONTEXT ( 3 ) GLOBAL_UNCERTAINTY_ASSIGNED_CONTEXT ( ( #3018 ) ) GLOBAL_UNIT_ASSIGNED_CONTEXT ( ( #13477, #13562, #4697 ) ) REPRESENTATION_CONTEXT ( 'NONE', 'WORKASPACE' ) );
#10939 = ORIENTED_EDGE ( 'NONE', *, *, #5000, .F. ) ;
#10940 = CARTESIAN_POINT ( 'NONE',  ( -2.131511515620587272, -3.916244202832140253, -4.937499998634406140 ) ) ;
#10941 = SURFACE_STYLE_FILL_AREA ( #1154 ) ;
#10942 = CARTESIAN_POINT ( 'NONE',  ( 0.5093500532425063732, 4.799145180956616130, -8.124999998634407916 ) ) ;
#10943 = DIRECTION ( 'NONE',  ( 0.000000000000000000, 0.000000000000000000, 1.000000000000000000 ) ) ;
#10944 = DIRECTION ( 'NONE',  ( 0.8660254037844381525, -0.5000000000000007772, 0.000000000000000000 ) ) ;
#10945 = ADVANCED_FACE ( 'NONE', ( #1870 ), #10061, .T. ) ;
#10946 = DIRECTION ( 'NONE',  ( 0.8660254037844389297, -0.000000000000000000, -0.4999999999999997780 ) ) ;
#10947 = COLOUR_RGB ( '', 0.31764706, 0.68627451, 0.89019608) ;
#10948 = CARTESIAN_POINT ( 'NONE',  ( -1.415196051561583790, 4.795541693661363958, 0.3750000027311836681 ) ) ;
#10949 = SURFACE_STYLE_FILL_AREA ( #14585 ) ;
#10950 = CARTESIAN_POINT ( 'NONE',  ( -1.846868145590734756, -25.37500000136559564, -4.458734124999999437 ) ) ;
#10951 = VECTOR ( 'NONE', #10018, 1000.000000000000000 ) ;
#10952 = CARTESIAN_POINT ( 'NONE',  ( 3.033343224707661712, -3.753672977998669946, -4.499999998634407028 ) ) ;
#10953 = CARTESIAN_POINT ( 'NONE',  ( -60.00000000000000000, -37.00000000000000711, 19.99999999999999289 ) ) ;
#10954 = ORIENTED_EDGE ( 'NONE', *, *, #11179, .F. ) ;
#10955 = ORIENTED_EDGE ( 'NONE', *, *, #12598, .T. ) ;
#10956 = EDGE_LOOP ( 'NONE', ( #10410, #4640 ) ) ;
#10957 = CARTESIAN_POINT ( 'NONE',  ( -4.458734125000000326, -23.25000000136559208, -1.846868145590735644 ) ) ;
#10958 = DIRECTION ( 'NONE',  ( 0.000000000000000000, 1.000000000000000000, 0.000000000000000000 ) ) ;
#10959 = DIRECTION ( 'NONE',  ( -0.5000000000000005551, -0.000000000000000000, 0.8660254037844382635 ) ) ;
#10960 = B_SPLINE_CURVE_WITH_KNOTS ( 'NONE', 3,
 ( #6193, #14508, #1085, #15889, #3430, #6024 ),
 .UNSPECIFIED., .F., .F.,
 ( 4, 2, 4 ),
 ( 0.000000000000000000, 0.0004189869898914128608, 0.0008379739797828257217 ),
 .UNSPECIFIED. ) ;
#10961 = AXIS2_PLACEMENT_3D ( 'NONE', #8476, #952, #9904 ) ;
#10962 = ADVANCED_FACE ( 'NONE', ( #4393 ), #3172, .T. ) ;
#10963 = CARTESIAN_POINT ( 'NONE',  ( -91.33974596215558961, -105.7735026918962546, 7.500000000000001776 ) ) ;
#10964 = FACE_OUTER_BOUND ( 'NONE', #6962, .T. ) ;
#10965 = EDGE_CURVE ( 'NONE', #9262, #10093, #1266, .T. ) ;
#10966 = EDGE_CURVE ( 'NONE', #8519, #14655, #14038, .T. ) ;
#10967 = CARTESIAN_POINT ( 'NONE',  ( 19.99999999999956657, -8.786575603324269439E-13, 0.000000000000000000 ) ) ;
#10968 = CARTESIAN_POINT ( 'NONE',  ( 3.401574460001763001, -4.209348295687703967, -3.187500000000003553 ) ) ;
#10969 = CARTESIAN_POINT ( 'NONE',  ( 0.000000000000000000, -20.00000000000000000, 5.000000000000000000 ) ) ;
#10970 = CARTESIAN_POINT ( 'NONE',  ( 0.000000000000000000, -20.00000000000000000, 1.500000000000000000 ) ) ;
#10971 = CARTESIAN_POINT ( 'NONE',  ( -3.152801135295367985, -27.81250000136559564, 3.152801135295367096 ) ) ;
#10972 =( GEOMETRIC_REPRESENTATION_CONTEXT ( 3 ) GLOBAL_UNCERTAINTY_ASSIGNED_CONTEXT ( ( #10313 ) ) GLOBAL_UNIT_ASSIGNED_CONTEXT ( ( #5272, #11571, #15138 ) ) REPRESENTATION_CONTEXT ( 'NONE', 'WORKASPACE' ) );
#10973 =( BOUNDED_CURVE ( )  B_SPLINE_CURVE ( 2, ( #2955, #2634, #7759, #240, #6372, #10089, #8875, #5159, #7829 ),
 .UNSPECIFIED., .F., .F. ) 
 B_SPLINE_CURVE_WITH_KNOTS ( ( 3, 2, 2, 2, 3 ),
 ( 0.1750000000000001554, 0.1875000000000001665, 0.2000000000000001776, 0.2125000000000001887, 0.2250000000000001998 ),
 .UNSPECIFIED. ) 
 CURVE ( )  GEOMETRIC_REPRESENTATION_ITEM ( )  RATIONAL_B_SPLINE_CURVE ( ( 0.9999999999999990008, 0.9238795325112877377, 1.000000000000000000, 0.9238795325112867385, 1.000000000000000000, 0.9238795325112867385, 1.000000000000000000, 0.9238795325112855172, 1.000000000000001110 ) ) 
 REPRESENTATION_ITEM ( '' )  );
#10974 = CARTESIAN_POINT ( 'NONE',  ( -2.131511515620587272, -3.916244202832140253, -2.937499998634407472 ) ) ;
#10975 = ORIENTED_EDGE ( 'NONE', *, *, #10733, .T. ) ;
#10976 = MECHANICAL_DESIGN_GEOMETRIC_PRESENTATION_REPRESENTATION (  '', ( #9173 ), #11981 ) ;
#10977 = DIRECTION ( 'NONE',  ( 0.000000000000000000, 0.000000000000000000, -1.000000000000000000 ) ) ;
#10978 = ORIENTED_EDGE ( 'NONE', *, *, #11590, .T. ) ;
#10979 = ORIENTED_EDGE ( 'NONE', *, *, #9462, .T. ) ;
#10981 = CARTESIAN_POINT ( 'NONE',  ( -4.000000000000000000, -2.309401076758512694, -3.433295621305382461 ) ) ;
#10980 = COLOUR_RGB ( '', 0.31764706, 0.68627451, 0.89019608) ;
#10982 = CARTESIAN_POINT ( 'NONE',  ( 4.458734124999999437, -23.50000000136559564, 1.846868145590737864 ) ) ;
#10983 = CARTESIAN_POINT ( 'NONE',  ( 2.500000000000000000, 3.004629197474318851E-15, 2.042000000000000259 ) ) ;
#10984 = ORIENTED_EDGE ( 'NONE', *, *, #5416, .T. ) ;
#10985 = CARTESIAN_POINT ( 'NONE',  ( 0.000000000000000000, -20.00000000000000000, 5.000000000000000000 ) ) ;
#10986 = VECTOR ( 'NONE', #737, 1000.000000000000000 ) ;
#10987 = CARTESIAN_POINT ( 'NONE',  ( -39.99999999999999289, -11.00000000000000178, -2.500000000000079492 ) ) ;
#10988 = CARTESIAN_POINT ( 'NONE',  ( -1.654252653721913102, -3.663718938583024443, -0.01223254789874440342 ) ) ;
#10989 = CARTESIAN_POINT ( 'NONE',  ( 5.000000000000004441, 3.034671531081452754E-15, -0.9202630448617579173 ) ) ;
#10990 = CIRCLE ( 'NONE', #1175, 10.00000000000000000 ) ;
#10991 = ADVANCED_FACE ( 'NONE', ( #13564 ), #11004, .T. ) ;
#10992 = CARTESIAN_POINT ( 'NONE',  ( 4.458734125000000326, -23.62500000136559919, -1.846868145590734978 ) ) ;
#10993 = CIRCLE ( 'NONE', #6088, 1.999999999999998224 ) ;
#10994 = DIRECTION ( 'NONE',  ( -0.4999999999999997224, -0.000000000000000000, -0.8660254037844388186 ) ) ;
#10995 = DIRECTION ( 'NONE',  ( 1.000000000000000000, 0.000000000000000000, 0.000000000000000000 ) ) ;
#10996 = CARTESIAN_POINT ( 'NONE',  ( -2.071067811865478170, -27.43750000273119127, 5.000000000000000000 ) ) ;
#10997 = CARTESIAN_POINT ( 'NONE',  ( 5.000000000000002665, 1.275685995473128912E-14, -5.920263044861758139 ) ) ;
#10998 = CARTESIAN_POINT ( 'NONE',  ( 5.000000000000004441, -2.247904837838113790E-16, -7.045263047592947636 ) ) ;
#10999 = DIRECTION ( 'NONE',  ( 0.000000000000000000, 1.000000000000000000, 0.000000000000000000 ) ) ;
#11000 = ORIENTED_EDGE ( 'NONE', *, *, #5683, .T. ) ;
#11001 = AXIS2_PLACEMENT_3D ( 'NONE', #1410, #15895, #8861 ) ;
#11002 =( NAMED_UNIT ( * ) PLANE_ANGLE_UNIT ( ) SI_UNIT ( $, .RADIAN. ) );
#11003 = ORIENTED_EDGE ( 'NONE', *, *, #3334, .F. ) ;
#11004 = CYLINDRICAL_SURFACE ( 'NONE', #7480, 32.00000000000000000 ) ;
#11005 = CIRCLE ( 'NONE', #7664, 10.00000000000000000 ) ;
#11006 = ORIENTED_EDGE ( 'NONE', *, *, #12620, .T. ) ;
#11007 = AXIS2_PLACEMENT_3D ( 'NONE', #7638, #3898, #6337 ) ;
#11008 = DIRECTION ( 'NONE',  ( 0.000000000000000000, 0.000000000000000000, 1.000000000000000000 ) ) ;
#11009 = CIRCLE ( 'NONE', #10539, 5.000000000000001776 ) ;
#11010 = CARTESIAN_POINT ( 'NONE',  ( 5.000000000000000888, 0.000000000000000000, -25.03750572909317285 ) ) ;
#11011 = CARTESIAN_POINT ( 'NONE',  ( 0.5093500532425063732, 4.799145180956616130, 0.8750000013655920839 ) ) ;
#11012 = CARTESIAN_POINT ( 'NONE',  ( -6.768483173307416678E-13, 32.00000000000000000, 67.49999999999930367 ) ) ;
#11013 = AXIS2_PLACEMENT_3D ( 'NONE', #11196, #382, #140 ) ;
#11014 = CARTESIAN_POINT ( 'NONE',  ( -3.033343224707664376, 3.753672977998667726, -3.249999998634409692 ) ) ;
#11015 = CARTESIAN_POINT ( 'NONE',  ( 0.2500000000000002220, 4.898587196589412829E-16, -4.000000000000000000 ) ) ;
#11016 = FILL_AREA_STYLE_COLOUR ( '', #7964 ) ;
#11017 = LINE ( 'NONE', #12209, #7973 ) ;
#11018 = SHAPE_REPRESENTATION_RELATIONSHIP ( 'NONE' , 'NONE' ,  #14733, #9085 ) ;
#11019 = EDGE_LOOP ( 'NONE', ( #12277, #1045 ) ) ;
#11020 = CARTESIAN_POINT ( 'NONE',  ( 4.000000000000000000, 1.680228229147133767, -3.316631783032546021 ) ) ;
#11021 = VECTOR ( 'NONE', #467, 1000.000000000000000 ) ;
#11022 = ORIENTED_EDGE ( 'NONE', *, *, #6200, .F. ) ;
#11023 = ORIENTED_EDGE ( 'NONE', *, *, #5359, .T. ) ;
#11024 = CARTESIAN_POINT ( 'NONE',  ( -2.131511515620587272, -3.916244202832140253, -2.937499998634407472 ) ) ;
#11025 = EDGE_CURVE ( 'NONE', #12457, #3698, #9795, .T. ) ;
#11026 = EDGE_CURVE ( 'NONE', #13189, #11827, #9865, .T. ) ;
#11027 = CARTESIAN_POINT ( 'NONE',  ( 4.458734124999999437, -22.43750000136559564, 0.000000000000000000 ) ) ;
#11028 = DIRECTION ( 'NONE',  ( 0.000000000000000000, 1.000000000000000000, 0.000000000000000000 ) ) ;
#11029 = CARTESIAN_POINT ( 'NONE',  ( -39.99999999999999289, -9.000000000000001776, 2.500000000001739497 ) ) ;
#11030 = DIRECTION ( 'NONE',  ( -1.000000000000000000, 0.000000000000000000, 1.239088197126290570E-16 ) ) ;
#11032 = CARTESIAN_POINT ( 'NONE',  ( 12.67949192431126093, -4.999999999999997335, -61.96152422706632024 ) ) ;
#11031 = VECTOR ( 'NONE', #6931, 1000.000000000000000 ) ;
#11033 = DIRECTION ( 'NONE',  ( 0.000000000000000000, 0.000000000000000000, 1.000000000000000000 ) ) ;
#11034 = FACE_OUTER_BOUND ( 'NONE', #4350, .T. ) ;
#11035 = CARTESIAN_POINT ( 'NONE',  ( -2.071067811865489272, -22.81250000273118417, -4.999999999999985789 ) ) ;
#11036 = CARTESIAN_POINT ( 'NONE',  ( -3.152801135295367096, -24.31250000136559564, -3.152801135295367541 ) ) ;
#11037 = CARTESIAN_POINT ( 'NONE',  ( 1.846868145590736310, -22.62500000136559564, 4.458734124999997661 ) ) ;
#11038 = CARTESIAN_POINT ( 'NONE',  ( -2.131511515620587272, -3.916244202832140253, -4.687499998634405252 ) ) ;
#11039 = VECTOR ( 'NONE', #12037, 1000.000000000000000 ) ;
#11040 = DIRECTION ( 'NONE',  ( -0.8660254037844390407, 0.000000000000000000, 0.4999999999999993339 ) ) ;
#11041 = VERTEX_POINT ( 'NONE', #9944 ) ;
#11042 = ORIENTED_EDGE ( 'NONE', *, *, #9886, .F. ) ;
#11043 = DIRECTION ( 'NONE',  ( 0.000000000000000000, 0.000000000000000000, 1.000000000000000000 ) ) ;
#11044 = VERTEX_POINT ( 'NONE', #3804 ) ;
#11045 = CARTESIAN_POINT ( 'NONE',  ( 2.730187237215162345E-16, -24.43750000136559564, -4.458734124999999437 ) ) ;
#11046 = EDGE_CURVE ( 'NONE', #11740, #1580, #10567, .T. ) ;
#11047 = CARTESIAN_POINT ( 'NONE',  ( -9.184850993605147944E-16, -23.37500000273118772, 5.000000000000000000 ) ) ;
#11048 = EDGE_CURVE ( 'NONE', #3061, #11169, #10920, .T. ) ;
#11049 = CARTESIAN_POINT ( 'NONE',  ( -3.535533905932737309, -27.75000000273118772, -3.535533905932738197 ) ) ;
#11050 =( REPRESENTATION_RELATIONSHIP ('NONE','NONE', #4176, #4696 ) REPRESENTATION_RELATIONSHIP_WITH_TRANSFORMATION ( #11806 )SHAPE_REPRESENTATION_RELATIONSHIP( ) );
#11051 = VECTOR ( 'NONE', #977, 1000.000000000000000 ) ;
#11052 = LINE ( 'NONE', #13216, #6892 ) ;
#11053 = CARTESIAN_POINT ( 'NONE',  ( -91.33974596215557540, -105.7735026918962689, 17.50000000000000000 ) ) ;
#11054 = CARTESIAN_POINT ( 'NONE',  ( 6.000000000000000000, -13.00000000000000178, 1.500000000000000000 ) ) ;
#11055 = CARTESIAN_POINT ( 'NONE',  ( 1.415196051561583790, -4.795541693661363958, -3.250000000000002665 ) ) ;
#11056 = CARTESIAN_POINT ( 'NONE',  ( 4.999999999999849898, -1.272547481429010530, -1.961597479913463449 ) ) ;
#11057 = STYLED_ITEM ( 'NONE', ( #9819 ), #9140 ) ;
#11058 = CARTESIAN_POINT ( 'NONE',  ( -3.535533905932738641, -27.37500000000000000, 3.535533905932737309 ) ) ;
#11059 = CARTESIAN_POINT ( 'NONE',  ( 2.730187237215162345E-16, -27.18750000136559564, -4.458734124999999437 ) ) ;
#11060 = VECTOR ( 'NONE', #14098, 1000.000000000000000 ) ;
#11061 = CARTESIAN_POINT ( 'NONE',  ( 4.799145180956616130, -0.5093500532425063732, -3.624999998634407916 ) ) ;
#11062 = ORIENTED_EDGE ( 'NONE', *, *, #11048, .T. ) ;
#11063 = LINE ( 'NONE', #3695, #4803 ) ;
#11064 = VERTEX_POINT ( 'NONE', #6073 ) ;
#11065 = ORIENTED_EDGE ( 'NONE', *, *, #14598, .F. ) ;
#11066 = CARTESIAN_POINT ( 'NONE',  ( -7.915341292091955694, -3.857523022641926591, -7.913710289177963375 ) ) ;
#11067 = CARTESIAN_POINT ( 'NONE',  ( 1.846868145590735200, -26.25000000136559208, -4.458734125000000326 ) ) ;
#11068 = EDGE_CURVE ( 'NONE', #11174, #15077, #4865, .T. ) ;
#11069 = DIRECTION ( 'NONE',  ( -1.000000000000000000, 0.000000000000000000, 0.000000000000000000 ) ) ;
#11070 = ADVANCED_FACE ( 'NONE', ( #12123 ), #3721, .F. ) ;
#11071 = ORIENTED_EDGE ( 'NONE', *, *, #3634, .F. ) ;
#11072 = CARTESIAN_POINT ( 'NONE',  ( -124.9999999999999858, -115.2072594216369907, 17.50000000000000000 ) ) ;
#11073 = CIRCLE ( 'NONE', #11568, 57.99999999999999289 ) ;
#11074 = AXIS2_PLACEMENT_3D ( 'NONE', #12111, #7355, #6148 ) ;
#11075 = DIRECTION ( 'NONE',  ( 0.000000000000000000, -1.000000000000000000, 1.471414886128461471E-15 ) ) ;
#11076 = CARTESIAN_POINT ( 'NONE',  ( 2.500000000000000000, 1.178949249685213863, -2.042000000000001148 ) ) ;
#11077 = DIRECTION ( 'NONE',  ( 0.000000000000000000, 1.000000000000000000, 0.000000000000000000 ) ) ;
#11078 =( BOUNDED_CURVE ( )  B_SPLINE_CURVE ( 3, ( #7585, #1589, #15016, #11290 ),
 .UNSPECIFIED., .F., .F. ) 
 B_SPLINE_CURVE_WITH_KNOTS ( ( 4, 4 ),
 ( 1.570796326794896780, 3.141592653589793116 ),
 .UNSPECIFIED. ) 
 CURVE ( )  GEOMETRIC_REPRESENTATION_ITEM ( )  RATIONAL_B_SPLINE_CURVE ( ( 1.000000000000000000, 0.8047378541243650485, 0.8047378541243650485, 1.000000000000000000 ) ) 
 REPRESENTATION_ITEM ( '' )  );
#11079 = CARTESIAN_POINT ( 'NONE',  ( -3.152801135295367096, -22.31250000136559564, -3.152801135295367541 ) ) ;
#11080 = CARTESIAN_POINT ( 'NONE',  ( 0.000000000000000000, 0.000000000000000000, 0.000000000000000000 ) ) ;
#11081 = DIRECTION ( 'NONE',  ( 0.000000000000000000, 0.000000000000000000, 1.000000000000000000 ) ) ;
#11082 = CARTESIAN_POINT ( 'NONE',  ( -2.071067811865475061, -28.81250000273118772, -5.000000000000000888 ) ) ;
#11083 = CARTESIAN_POINT ( 'NONE',  ( -28.86751345948129455, 0.000000000000000000, 49.99999999999999289 ) ) ;
#11084 = CARTESIAN_POINT ( 'NONE',  ( -3.152801135295367096, -30.06250000136559564, -3.152801135295367541 ) ) ;
#11085 = ORIENTED_EDGE ( 'NONE', *, *, #3298, .T. ) ;
#11086 = VECTOR ( 'NONE', #8042, 1000.000000000000000 ) ;
#11087 = VERTEX_POINT ( 'NONE', #7539 ) ;
#11088 = CARTESIAN_POINT ( 'NONE',  ( -19.99999999999956657, -9.000000000000001776, 2.500000000000877520 ) ) ;
#11089 = EDGE_CURVE ( 'NONE', #11044, #3131, #9151, .T. ) ;
#11090 = ORIENTED_EDGE ( 'NONE', *, *, #10156, .T. ) ;
#11091 = DIRECTION ( 'NONE',  ( 0.000000000000000000, 1.000000000000000000, 0.000000000000000000 ) ) ;
#11092 = CARTESIAN_POINT ( 'NONE',  ( -2.071067811865489272, -25.81250000273118417, -4.999999999999985789 ) ) ;
#11093 = CARTESIAN_POINT ( 'NONE',  ( -3.916244202832140253, 2.131511515620587272, -2.937499998634407472 ) ) ;
#11094 = PRODUCT_CONTEXT ( 'NONE', #9192, 'mechanical' ) ;
#11095 = CARTESIAN_POINT ( 'NONE',  ( 4.799145180956616130, -0.5093500532425063732, -3.624999998634407916 ) ) ;
#11096 = DIRECTION ( 'NONE',  ( 1.000000000000000000, 0.000000000000000000, 0.000000000000000000 ) ) ;
#11097 = DIRECTION ( 'NONE',  ( -0.4999999999999966138, -0.8660254037844405950, 0.000000000000000000 ) ) ;
#11098 = CARTESIAN_POINT ( 'NONE',  ( -28.86751345948130165, -37.00000000000000711, 20.00000000000000355 ) ) ;
#11099 = ORIENTED_EDGE ( 'NONE', *, *, #2188, .F. ) ;
#11100 = DIRECTION ( 'NONE',  ( -0.000000000000000000, 1.000000000000000000, -0.000000000000000000 ) ) ;
#11101 = DIRECTION ( 'NONE',  ( 0.9999824063907752913, 0.005931855436079607087, 0.000000000000000000 ) ) ;
#11102 = EDGE_CURVE ( 'NONE', #9435, #7272, #14350, .T. ) ;
#11103 = ORIENTED_EDGE ( 'NONE', *, *, #1486, .F. ) ;
#11104 = CARTESIAN_POINT ( 'NONE',  ( 2.131511515620586383, 3.916244202832140253, -2.437499998634407028 ) ) ;
#11105 = FILL_AREA_STYLE_COLOUR ( '', #10980 ) ;
#11106 = CARTESIAN_POINT ( 'NONE',  ( -35.00000000000000000, 40.00000000000000000, 2.649999999999992806 ) ) ;
#11107 = CARTESIAN_POINT ( 'NONE',  ( -1.206569728928479579, -7.963640680051486953, -0.4524126574264535905 ) ) ;
#11108 = FACE_OUTER_BOUND ( 'NONE', #219, .T. ) ;
#11109 = CARTESIAN_POINT ( 'NONE',  ( -4.391654775818395251, 2.390265326283148806, 0.5000000027311837236 ) ) ;
#11110 = CARTESIAN_POINT ( 'NONE',  ( 25.00000000000000000, 2.055000000000000160, 0.000000000000000000 ) ) ;
#11111 = EDGE_CURVE ( 'NONE', #7180, #11920, #7458, .T. ) ;
#11112 = CYLINDRICAL_SURFACE ( 'NONE', #493, 3.499999999999999556 ) ;
#11113 = CARTESIAN_POINT ( 'NONE',  ( -4.458734125000000326, -26.12500000136559919, 1.846868145590734089 ) ) ;
#11114 = CARTESIAN_POINT ( 'NONE',  ( 3.152801135295366208, -21.56250000136559208, 3.152801135295367985 ) ) ;
#11115 = CARTESIAN_POINT ( 'NONE',  ( 4.276409079477644148, 1.261996585732577891, -4.312499998634405252 ) ) ;
#11116 = CARTESIAN_POINT ( 'NONE',  ( -4.154094228333456762, 2.398367420968013253, -3.721909803043220055 ) ) ;
#11117 = VERTEX_POINT ( 'NONE', #12364 ) ;
#11118 = VERTEX_POINT ( 'NONE', #8436 ) ;
#11119 = DIRECTION ( 'NONE',  ( 1.000000000000000000, 0.000000000000000000, 0.000000000000000000 ) ) ;
#11120 = ORIENTED_EDGE ( 'NONE', *, *, #11812, .T. ) ;
#11121 = CARTESIAN_POINT ( 'NONE',  ( 4.458734125000000326, -23.62500000136559919, -1.846868145590734978 ) ) ;
#11122 = DIRECTION ( 'NONE',  ( -0.000000000000000000, 1.000000000000000000, -0.000000000000000000 ) ) ;
#11123 = PLANE ( 'NONE',  #6903 ) ;
#11124 = LINE ( 'NONE', #4668, #14516 ) ;
#11125 = LINE ( 'NONE', #4984, #13122 ) ;
#11126 = CARTESIAN_POINT ( 'NONE',  ( -3.401574460001764777, 4.209348295687701302, 0.3124999999999955591 ) ) ;
#11127 = FACE_OUTER_BOUND ( 'NONE', #14721, .T. ) ;
#11128 = EDGE_CURVE ( 'NONE', #13637, #2243, #15386, .T. ) ;
#11129 = CARTESIAN_POINT ( 'NONE',  ( -2.319649502132982821, -4.215050057573432873, -0.1373479633058615201 ) ) ;
#11130 = ADVANCED_FACE ( 'NONE', ( #2271 ), #7222, .T. ) ;
#11131 = CARTESIAN_POINT ( 'NONE',  ( 2.730187237215162345E-16, -25.18750000136559564, -4.458734124999999437 ) ) ;
#11132 = CARTESIAN_POINT ( 'NONE',  ( 3.033343224707661712, -3.753672977998669946, -1.749999998634408360 ) ) ;
#11133 = ORIENTED_EDGE ( 'NONE', *, *, #10879, .F. ) ;
#11134 = CARTESIAN_POINT ( 'NONE',  ( 3.750000000000005773, 6.495190528383288253, 0.000000000000000000 ) ) ;
#11135 = ORIENTED_EDGE ( 'NONE', *, *, #14466, .T. ) ;
#11136 = ORIENTED_EDGE ( 'NONE', *, *, #6671, .T. ) ;
#11137 = DIRECTION ( 'NONE',  ( 0.8660254037844388186, 0.000000000000000000, -0.4999999999999997224 ) ) ;
#11138 = CARTESIAN_POINT ( 'NONE',  ( 4.458734124999999437, -26.43750000136559564, 0.000000000000000000 ) ) ;
#11139 = DIRECTION ( 'NONE',  ( 0.000000000000000000, 0.000000000000000000, 1.000000000000000000 ) ) ;
#11140 = ORIENTED_EDGE ( 'NONE', *, *, #9945, .T. ) ;
#11141 = CARTESIAN_POINT ( 'NONE',  ( -94.99999999999994316, -103.6602540378444246, 17.50000000000000000 ) ) ;
#11142 = CARTESIAN_POINT ( 'NONE',  ( 1.305263714129178299, -8.377797850839291627, -7.792447862505336609 ) ) ;
#11143 = CARTESIAN_POINT ( 'NONE',  ( 0.000000000000000000, 40.00000000000000000, 0.000000000000000000 ) ) ;
#11144 = DIRECTION ( 'NONE',  ( -1.000000000000000000, -0.000000000000000000, -1.114413700119375779E-16 ) ) ;
#11145 = CARTESIAN_POINT ( 'NONE',  ( 5.000000000000000000, -31.06250000000000000, 2.071067811865478614 ) ) ;
#11146 = CARTESIAN_POINT ( 'NONE',  ( 10.12668159690567649, 0.000000000000000000, -9.999999999999998224 ) ) ;
#11147 = ADVANCED_FACE ( 'NONE', ( #9704 ), #15859, .F. ) ;
#11148 = DIRECTION ( 'NONE',  ( 1.000000000000000000, 0.000000000000000000, -0.000000000000000000 ) ) ;
#11149 = ADVANCED_FACE ( 'NONE', ( #3886 ), #6404, .F. ) ;
#11150 = CARTESIAN_POINT ( 'NONE',  ( -5.000000000000000888, -27.56250000273118772, 2.071067811865474617 ) ) ;
#11151 = CARTESIAN_POINT ( 'NONE',  ( 0.6508621380849223259, 8.763657152406455708, -7.907633014911222169 ) ) ;
#11152 = CARTESIAN_POINT ( 'NONE',  ( -1.846868145590737420, -28.75000000136559564, 4.458734124999997661 ) ) ;
#11153 = CARTESIAN_POINT ( 'NONE',  ( 11.45098066423670247, 0.000000000000000000, 1.122567565269603304E-11 ) ) ;
#11154 = ORIENTED_EDGE ( 'NONE', *, *, #14294, .T. ) ;
#11155 = ORIENTED_EDGE ( 'NONE', *, *, #13618, .F. ) ;
#11156 = CARTESIAN_POINT ( 'NONE',  ( -0.6507732100473471171, 4.243078065514775510, -0.2236248678334823436 ) ) ;
#11157 = ORIENTED_EDGE ( 'NONE', *, *, #1094, .F. ) ;
#11158 = DIRECTION ( 'NONE',  ( 1.000000000000000000, 0.000000000000000000, 0.000000000000000000 ) ) ;
#11159 = CARTESIAN_POINT ( 'NONE',  ( -3.535533905932737309, -25.75000000273118417, -3.535533905932738197 ) ) ;
#11160 = ADVANCED_FACE ( 'NONE', ( #13903 ), #8426, .F. ) ;
#11161 = CARTESIAN_POINT ( 'NONE',  ( 4.276409079477644148, 1.261996585732577891, -3.312499998634407916 ) ) ;
#11162 = EDGE_CURVE ( 'NONE', #13611, #5349, #7382, .T. ) ;
#11163 = SHAPE_DEFINITION_REPRESENTATION ( #13373, #15130 ) ;
#11164 = EDGE_CURVE ( 'NONE', #3645, #928, #14338, .T. ) ;
#11165 = CARTESIAN_POINT ( 'NONE',  ( -0.5093500532425060401, -4.799145180956616130, -5.874999998634406140 ) ) ;
#11166 = CARTESIAN_POINT ( 'NONE',  ( 4.197393957002303999, 0.8151795401431359833, -3.503767560748935139 ) ) ;
#11167 = DIRECTION ( 'NONE',  ( 0.5000000000000002220, 0.000000000000000000, -0.8660254037844383745 ) ) ;
#11168 = VECTOR ( 'NONE', #572, 1000.000000000000000 ) ;
#11169 = VERTEX_POINT ( 'NONE', #15047 ) ;
#11170 = CARTESIAN_POINT ( 'NONE',  ( 4.790360200640285449, -4.342938577510797593, -48.50984154344460109 ) ) ;
#11171 = ORIENTED_EDGE ( 'NONE', *, *, #6341, .F. ) ;
#11172 = DIRECTION ( 'NONE',  ( 0.000000000000000000, 0.000000000000000000, -1.000000000000000000 ) ) ;
#11173 = VECTOR ( 'NONE', #13472, 1000.000000000000000 ) ;
#11174 = VERTEX_POINT ( 'NONE', #15120 ) ;
#11175 = CARTESIAN_POINT ( 'NONE',  ( -3.033343224707664820, 3.753672977998667726, -2.249999998634408804 ) ) ;
#11176 = DIRECTION ( 'NONE',  ( -0.000000000000000000, -1.000000000000000000, -0.000000000000000000 ) ) ;
#11177 = CARTESIAN_POINT ( 'NONE',  ( 42.02221399786069611, 0.000000000000000000, 1.075528555105620399E-13 ) ) ;
#11178 = CARTESIAN_POINT ( 'NONE',  ( -2.452879891156813041, -7.244083172395187731, -0.1007566405101838203 ) ) ;
#11179 = EDGE_CURVE ( 'NONE', #3171, #2621, #12772, .T. ) ;
#11180 = CARTESIAN_POINT ( 'NONE',  ( 3.535533905932738197, -27.00000000273118772, -3.535533905932738197 ) ) ;
#11181 = CARTESIAN_POINT ( 'NONE',  ( -4.391654775818395251, 2.390265326283148806, -2.499999997268815388 ) ) ;
#11182 = DIRECTION ( 'NONE',  ( 0.000000000000000000, -1.000000000000000000, -0.000000000000000000 ) ) ;
#11183 = CYLINDRICAL_SURFACE ( 'NONE', #2025, 1.999999999999998224 ) ;
#11185 = CIRCLE ( 'NONE', #4224, 2.649999999999992806 ) ;
#11184 = CARTESIAN_POINT ( 'NONE',  ( 1.846868145590736310, -23.87500000136559564, 4.458734124999997661 ) ) ;
#11186 = ORIENTED_EDGE ( 'NONE', *, *, #12350, .T. ) ;
#11187 = CYLINDRICAL_SURFACE ( 'NONE', #10788, 2.649999999999999467 ) ;
#11188 = CARTESIAN_POINT ( 'NONE',  ( 3.033343224707661712, -3.753672977998669946, -2.499999998634408804 ) ) ;
#11189 = CYLINDRICAL_SURFACE ( 'NONE', #5057, 2.100000000000000089 ) ;
#11190 = VERTEX_POINT ( 'NONE', #15291 ) ;
#11191 = ORIENTED_EDGE ( 'NONE', *, *, #10910, .T. ) ;
#11192 = CARTESIAN_POINT ( 'NONE',  ( 0.000000000000000000, 0.000000000000000000, 0.000000000000000000 ) ) ;
#11193 = VERTEX_POINT ( 'NONE', #12676 ) ;
#11194 = CARTESIAN_POINT ( 'NONE',  ( 4.458734124999999437, -24.68750000136559564, 0.000000000000000000 ) ) ;
#11195 = ADVANCED_FACE ( 'NONE', ( #1458 ), #510, .T. ) ;
#11196 = CARTESIAN_POINT ( 'NONE',  ( 0.000000000000000000, 40.00000000000000000, 0.000000000000000000 ) ) ;
#11197 = FACE_OUTER_BOUND ( 'NONE', #7594, .T. ) ;
#11198 = EDGE_CURVE ( 'NONE', #1925, #13370, #8841, .T. ) ;
#11199 = MECHANICAL_DESIGN_GEOMETRIC_PRESENTATION_REPRESENTATION (  '', ( #5009 ), #1137 ) ;
#11200 = CYLINDRICAL_SURFACE ( 'NONE', #15933, 2.649999999999992806 ) ;
#11201 = FACE_BOUND ( 'NONE', #3453, .T. ) ;
#11202 =( BOUNDED_CURVE ( )  B_SPLINE_CURVE ( 2, ( #3617, #6530, #11444, #5160, #7760, #11207, #2636, #1591, #7587 ),
 .UNSPECIFIED., .F., .F. ) 
 B_SPLINE_CURVE_WITH_KNOTS ( ( 3, 2, 2, 2, 3 ),
 ( 0.2749999999999999112, 0.2874999999999998668, 0.2999999999999999334, 0.3124999999999999445, 0.3249999999999999556 ),
 .UNSPECIFIED. ) 
 CURVE ( )  GEOMETRIC_REPRESENTATION_ITEM ( )  RATIONAL_B_SPLINE_CURVE ( ( 1.000000000000000666, 0.9238795325112860723, 1.000000000000000000, 0.9238795325112867385, 1.000000000000000000, 0.9238795325112867385, 1.000000000000000000, 0.9238795325112870716, 0.9999999999999996669 ) ) 
 REPRESENTATION_ITEM ( '' )  );
#11203 = CIRCLE ( 'NONE', #14560, 2.649999999999985700 ) ;
#11204 = DIRECTION ( 'NONE',  ( 0.8660254037844407060, -0.4999999999999965028, 0.000000000000000000 ) ) ;
#11205 = CARTESIAN_POINT ( 'NONE',  ( -1.415196051561583790, 4.795541693661363958, -4.750000000000000888 ) ) ;
#11206 = CARTESIAN_POINT ( 'NONE',  ( 1.415196051561583790, -4.795541693661363958, -2.124999997268814944 ) ) ;
#11207 = CARTESIAN_POINT ( 'NONE',  ( 5.000000000000000888, -28.93750000000000355, -2.071067811865475505 ) ) ;
#11208 = CARTESIAN_POINT ( 'NONE',  ( 1.846868145590735200, -26.25000000136559208, -4.458734125000000326 ) ) ;
#11209 = CARTESIAN_POINT ( 'NONE',  ( 3.753672977998667726, 3.033343224707664376, -4.499999998634407028 ) ) ;
#11210 = ORIENTED_EDGE ( 'NONE', *, *, #5204, .F. ) ;
#11211 = DIRECTION ( 'NONE',  ( -0.000000000000000000, -1.000000000000000000, -0.000000000000000000 ) ) ;
#11212 = ORIENTED_EDGE ( 'NONE', *, *, #14900, .F. ) ;
#11213 = EDGE_LOOP ( 'NONE', ( #9051, #3153, #5587, #4777, #1334 ) ) ;
#11214 = CARTESIAN_POINT ( 'NONE',  ( -4.000000000000000000, -0.8232339106130515116, -3.430630286862743183 ) ) ;
#11215 = AXIS2_PLACEMENT_3D ( 'NONE', #10927, #11329, #14893 ) ;
#11216 = CARTESIAN_POINT ( 'NONE',  ( -4.458734125000000326, -26.00000000136559208, -1.846868145590735644 ) ) ;
#11217 = DIRECTION ( 'NONE',  ( 0.000000000000000000, 0.000000000000000000, 1.000000000000000000 ) ) ;
#11218 = AXIS2_PLACEMENT_3D ( 'NONE', #14289, #11851, #798 ) ;
#11219 = EDGE_LOOP ( 'NONE', ( #11502, #6831, #2886, #4292 ) ) ;
#11220 = LINE ( 'NONE', #4022, #679 ) ;
#11221 = EDGE_CURVE ( 'NONE', #10129, #8029, #11322, .T. ) ;
#11222 = EDGE_CURVE ( 'NONE', #9532, #15211, #14599, .T. ) ;
#11223 = DIRECTION ( 'NONE',  ( -0.000000000000000000, -0.000000000000000000, 1.000000000000000000 ) ) ;
#11224 = CARTESIAN_POINT ( 'NONE',  ( 0.5093500532425063732, 4.799145180956616130, -2.124999998634406584 ) ) ;
#11225 = LINE ( 'NONE', #170, #4718 ) ;
#11226 = CIRCLE ( 'NONE', #943, 5.000000000000000000 ) ;
#11227 = CARTESIAN_POINT ( 'NONE',  ( 5.000000000000000000, -31.00000000000000000, 0.000000000000000000 ) ) ;
#11228 = CARTESIAN_POINT ( 'NONE',  ( 0.000000000000000000, 0.000000000000000000, -9.226681596905677907 ) ) ;
#11229 = LINE ( 'NONE', #3879, #1491 ) ;
#11230 = CARTESIAN_POINT ( 'NONE',  ( 3.535533905932736864, -29.25000000273118772, 3.535533905932738641 ) ) ;
#11231 = DIRECTION ( 'NONE',  ( 0.8660254037844383745, 0.000000000000000000, 0.5000000000000004441 ) ) ;
#11232 = DIRECTION ( 'NONE',  ( 0.000000000000000000, -0.8660254037844390407, -0.4999999999999994449 ) ) ;
#11233 = ORIENTED_EDGE ( 'NONE', *, *, #3313, .T. ) ;
#11234 = VERTEX_POINT ( 'NONE', #10037 ) ;
#11235 =( NAMED_UNIT ( * ) PLANE_ANGLE_UNIT ( ) SI_UNIT ( $, .RADIAN. ) );
#11236 = EDGE_LOOP ( 'NONE', ( #8724, #1892, #1911, #15226 ) ) ;
#11237 = CARTESIAN_POINT ( 'NONE',  ( 4.101954839143059139, -2.368264730582948285, -3.681130640444269631 ) ) ;
#11238 = AXIS2_PLACEMENT_3D ( 'NONE', #7036, #15682, #9677 ) ;
#11239 = ORIENTED_EDGE ( 'NONE', *, *, #5203, .T. ) ;
#11240 = DIRECTION ( 'NONE',  ( 0.000000000000000000, 0.000000000000000000, 1.000000000000000000 ) ) ;
#11241 = EDGE_CURVE ( 'NONE', #10374, #12492, #1619, .T. ) ;
#11242 = VECTOR ( 'NONE', #4760, 1000.000000000000000 ) ;
#11243 = VECTOR ( 'NONE', #12260, 1000.000000000000000 ) ;
#11244 = CARTESIAN_POINT ( 'NONE',  ( -1.846868145590734756, -31.37500000136559564, -4.458734125000000326 ) ) ;
#11245 = CARTESIAN_POINT ( 'NONE',  ( 1.261996585732578113, -4.276409079477644148, -2.562499998634407028 ) ) ;
#11246 =( NAMED_UNIT ( * ) PLANE_ANGLE_UNIT ( ) SI_UNIT ( $, .RADIAN. ) );
#11247 = VECTOR ( 'NONE', #7325, 1000.000000000000000 ) ;
#11248 = CARTESIAN_POINT ( 'NONE',  ( -4.799145180956616130, 0.5093500532425063732, -6.124999998634407916 ) ) ;
#11249 = CARTESIAN_POINT ( 'NONE',  ( 10.00000000000098765, -13.00000000000000178, 17.32050807568871065 ) ) ;
#11250 = DIRECTION ( 'NONE',  ( 0.2830392103123166025, -0.9591083387322728582, 0.000000000000000000 ) ) ;
#11251 = ORIENTED_EDGE ( 'NONE', *, *, #14488, .F. ) ;
#11252 = AXIS2_PLACEMENT_3D ( 'NONE', #2890, #6621, #10176 ) ;
#11253 = CARTESIAN_POINT ( 'NONE',  ( 3.007418566627519940, -3.000000000000001332, -48.95213768370648211 ) ) ;
#11254 = ORIENTED_EDGE ( 'NONE', *, *, #13061, .T. ) ;
#11255 = CARTESIAN_POINT ( 'NONE',  ( 57.73502691896258199, -37.00000000000000711, 2.081668171172168513E-14 ) ) ;
#11256 = DIRECTION ( 'NONE',  ( 0.000000000000000000, 0.000000000000000000, 1.000000000000000000 ) ) ;
#11257 = EDGE_LOOP ( 'NONE', ( #13407, #5256, #12973, #1831, #6253 ) ) ;
#11258 = CARTESIAN_POINT ( 'NONE',  ( -0.5093500532425060401, -4.799145180956616130, -5.874999998634406140 ) ) ;
#11259 = EDGE_CURVE ( 'NONE', #395, #742, #13732, .T. ) ;
#11260 = CIRCLE ( 'NONE', #1493, 25.00000000000000000 ) ;
#11261 = EDGE_CURVE ( 'NONE', #4540, #15603, #3619, .T. ) ;
#11262 = DIRECTION ( 'NONE',  ( -1.000000000000000000, 0.000000000000000000, 0.000000000000000000 ) ) ;
#11263 = AXIS2_PLACEMENT_3D ( 'NONE', #12958, #14269, #14196 ) ;
#11264 = DIRECTION ( 'NONE',  ( 0.000000000000000000, 0.000000000000000000, -1.000000000000000000 ) ) ;
#11265 = UNCERTAINTY_MEASURE_WITH_UNIT (LENGTH_MEASURE( 1.000000000000000082E-05 ), #1071, 'distance_accuracy_value', 'NONE');
#11266 = CARTESIAN_POINT ( 'NONE',  ( -81.33974596215558961, -105.7735026918962404, -7.500000000000000000 ) ) ;
#11267 = CARTESIAN_POINT ( 'NONE',  ( -2.390265326283148806, -4.391654775818394363, -5.249999997268817609 ) ) ;
#11268 = CARTESIAN_POINT ( 'NONE',  ( -44.43375672972994295, -3.000000000000000000, -19.99999999999594635 ) ) ;
#11269 = DIRECTION ( 'NONE',  ( 0.000000000000000000, 0.000000000000000000, 1.000000000000000000 ) ) ;
#11270 = CARTESIAN_POINT ( 'NONE',  ( 2.730187237215162345E-16, -23.43750000136559564, -4.458734124999999437 ) ) ;
#11271 = ORIENTED_EDGE ( 'NONE', *, *, #934, .T. ) ;
#11272 = DIRECTION ( 'NONE',  ( 1.000000000000000000, 0.000000000000000000, 3.343241100358131282E-16 ) ) ;
#11273 = CARTESIAN_POINT ( 'NONE',  ( 2.131511515620586383, 3.916244202832140253, -8.187499998634407916 ) ) ;
#11274 = CARTESIAN_POINT ( 'NONE',  ( -4.024497503033519941, 2.323544716729375459, -3.572167766733379768 ) ) ;
#11275 = ORIENTED_EDGE ( 'NONE', *, *, #13283, .F. ) ;
#11276 = EDGE_LOOP ( 'NONE', ( #675, #2560 ) ) ;
#11277 =( GEOMETRIC_REPRESENTATION_CONTEXT ( 3 ) GLOBAL_UNCERTAINTY_ASSIGNED_CONTEXT ( ( #123 ) ) GLOBAL_UNIT_ASSIGNED_CONTEXT ( ( #6249, #11246, #5192 ) ) REPRESENTATION_CONTEXT ( 'NONE', 'WORKASPACE' ) );
#11278 = AXIS2_PLACEMENT_3D ( 'NONE', #10437, #14066, #12844 ) ;
#11279 = CARTESIAN_POINT ( 'NONE',  ( 0.000000000000000000, 0.000000000000000000, 0.000000000000000000 ) ) ;
#11280 = ORIENTED_EDGE ( 'NONE', *, *, #1399, .F. ) ;
#11281 = VECTOR ( 'NONE', #9659, 1000.000000000000114 ) ;
#11282 = CARTESIAN_POINT ( 'NONE',  ( 4.999999999999849898, -1.272547481429012084, -0.08659748264465111367 ) ) ;
#11283 = ADVANCED_FACE ( 'NONE', ( #14234 ), #8103, .F. ) ;
#11284 = DIRECTION ( 'NONE',  ( 0.000000000000000000, 0.000000000000000000, 1.000000000000000000 ) ) ;
#11285 = AXIS2_PLACEMENT_3D ( 'NONE', #4959, #10063, #14993 ) ;
#11286 = FACE_OUTER_BOUND ( 'NONE', #7155, .T. ) ;
#11287 = CARTESIAN_POINT ( 'NONE',  ( -31.74999999999995737, 3.061616997868383634E-16, -2.500000000000000444 ) ) ;
#11288 = CARTESIAN_POINT ( 'NONE',  ( -90.00000000000000000, -95.00000000000000000, 17.50000000000000000 ) ) ;
#11289 = CARTESIAN_POINT ( 'NONE',  ( 3.401574460001763001, -4.209348295687703967, -5.187500000000001776 ) ) ;
#11290 = CARTESIAN_POINT ( 'NONE',  ( -44.99999999999999289, -35.00000000000000000, -7.500000000000000000 ) ) ;
#11291 = CARTESIAN_POINT ( 'NONE',  ( -19.99999999999956657, -13.00000000000000178, -2.499999999999120259 ) ) ;
#11292 = CARTESIAN_POINT ( 'NONE',  ( -1.846868145590737420, -28.75000000136559208, 4.458734124999999437 ) ) ;
#11293 = CARTESIAN_POINT ( 'NONE',  ( -4.799145180956616130, 0.5093500532425063732, -6.124999998634407916 ) ) ;
#11294 = ORIENTED_EDGE ( 'NONE', *, *, #5610, .T. ) ;
#11295 = AXIS2_PLACEMENT_3D ( 'NONE', #13152, #11860, #2087 ) ;
#11296 = CARTESIAN_POINT ( 'NONE',  ( 0.000000000000000000, 0.000000000000000000, 0.000000000000000000 ) ) ;
#11297 = EDGE_LOOP ( 'NONE', ( #15703, #10341, #10785 ) ) ;
#11298 = ORIENTED_EDGE ( 'NONE', *, *, #4198, .F. ) ;
#11299 = COLOUR_RGB ( '', 0.31764706, 0.68627451, 0.89019608) ;
#11300 = CARTESIAN_POINT ( 'NONE',  ( 1.846868145590736310, -24.62500000136559564, 4.458734124999999437 ) ) ;
#11301 = CARTESIAN_POINT ( 'NONE',  ( 0.000000000000000000, -13.00000000000000178, -6.000000000000000888 ) ) ;
#11302 = VERTEX_POINT ( 'NONE', #14468 ) ;
#11303 = VECTOR ( 'NONE', #843, 1000.000000000000000 ) ;
#11304 = CARTESIAN_POINT ( 'NONE',  ( -4.000000000000000000, 0.000000000000000000, 0.000000000000000000 ) ) ;
#11305 =( BOUNDED_SURFACE ( )  B_SPLINE_SURFACE ( 3, 2, ( 
 ( #4163, #8140, #11829 ),
 ( #1656, #15409, #15331 ),
 ( #5701, #8061, #463 ),
 ( #10328, #1739, #6689 ),
 ( #11597, #11747, #10396 ),
 ( #14109, #10566, #4333 ) ),
 .UNSPECIFIED., .F., .F., .F. ) 
 B_SPLINE_SURFACE_WITH_KNOTS ( ( 4, 2, 4 ),
 ( 3, 3 ),
 ( 0.02032853247518125531, 0.02278863295364820865, 0.02524873343211516200 ),
 ( 0.000000000000000000, 1.000000000000000000 ),
 .UNSPECIFIED. ) 
 GEOMETRIC_REPRESENTATION_ITEM ( )  RATIONAL_B_SPLINE_SURFACE ( (
 ( 1.000000000000000000, 0.8047781615896836271, 1.000000000000000000),
 ( 1.000000000000000000, 0.8123767586289967202, 1.000000000000000000),
 ( 1.000000000000000000, 0.8190662415563443322, 1.000000000000000000),
 ( 1.000000000000000000, 0.8192361015669982205, 1.000000000000000000),
 ( 1.000000000000000000, 0.8126135807103181952, 1.000000000000000000),
 ( 1.000000000000000000, 0.8047712338318587788, 1.000000000000000000) ) ) 
 REPRESENTATION_ITEM ( '' )  SURFACE ( )  );
#11306 = CARTESIAN_POINT ( 'NONE',  ( 5.276765049035075705, -6.073111908730306929, -7.634085501268428331 ) ) ;
#11307 = CARTESIAN_POINT ( 'NONE',  ( 4.799145180956616130, -0.5093500532425063732, -1.374999998634406140 ) ) ;
#11308 = CARTESIAN_POINT ( 'NONE',  ( 2.564533730342835938, 3.657148745220786257, -0.3789984458506786558 ) ) ;
#11309 = MECHANICAL_DESIGN_GEOMETRIC_PRESENTATION_REPRESENTATION (  '', ( #7720 ), #2523 ) ;
#11310 = CARTESIAN_POINT ( 'NONE',  ( -5.000000000000000888, -31.43750000000000355, 2.071067811865474617 ) ) ;
#11311 = DIRECTION ( 'NONE',  ( 1.000000000000000000, 0.000000000000000000, 0.000000000000000000 ) ) ;
#11312 = DIRECTION ( 'NONE',  ( 0.000000000000000000, 0.000000000000000000, 1.000000000000000000 ) ) ;
#11313 = CARTESIAN_POINT ( 'NONE',  ( -5.000000000000000000, -28.62500000273118772, -6.123233995736766282E-16 ) ) ;
#11314 = LINE ( 'NONE', #11625, #6013 ) ;
#11315 = CARTESIAN_POINT ( 'NONE',  ( 3.152801135295366208, -30.56250000136559564, 3.152801135295367985 ) ) ;
#11316 = EDGE_CURVE ( 'NONE', #15369, #6220, #1785, .T. ) ;
#11317 = VERTEX_POINT ( 'NONE', #4377 ) ;
#11318 = EDGE_LOOP ( 'NONE', ( #12275, #10496 ) ) ;
#11319 = ORIENTED_EDGE ( 'NONE', *, *, #6819, .T. ) ;
#11320 = CARTESIAN_POINT ( 'NONE',  ( 4.024499207728657879, -2.323545700935587988, -3.572172305156509964 ) ) ;
#11321 = VECTOR ( 'NONE', #8230, 1000.000000000000000 ) ;
#11322 = B_SPLINE_CURVE_WITH_KNOTS ( 'NONE', 3,
 ( #6483, #348, #11320, #11237, #7858, #15212 ),
 .UNSPECIFIED., .F., .F.,
 ( 4, 2, 4 ),
 ( 4.336808689942017736E-19, 0.0002095117440854729585, 0.0004190234881709454834 ),
 .UNSPECIFIED. ) ;
#11323 = CIRCLE ( 'NONE', #3068, 3.499999999999999556 ) ;
#11324 = EDGE_LOOP ( 'NONE', ( #13747, #6587, #7979 ) ) ;
#11325 = DIRECTION ( 'NONE',  ( 0.000000000000000000, 0.000000000000000000, -1.000000000000000000 ) ) ;
#11326 = AXIS2_PLACEMENT_3D ( 'NONE', #2688, #6343, #11580 ) ;
#11327 = CARTESIAN_POINT ( 'NONE',  ( 0.000000000000000000, 37.00000000000000000, 0.000000000000000000 ) ) ;
#11328 = CARTESIAN_POINT ( 'NONE',  ( 0.000000000000000000, 37.00000000000000000, 0.000000000000000000 ) ) ;
#11329 = DIRECTION ( 'NONE',  ( -3.061616997868408286E-17, 1.000000000000000000, -5.302876193624521016E-17 ) ) ;
#11330 = AXIS2_PLACEMENT_3D ( 'NONE', #5538, #1352, #1652 ) ;
#11331 = CARTESIAN_POINT ( 'NONE',  ( -4.799145180956616130, 0.5093500532425063732, -5.124999998634405252 ) ) ;
#11332 = DIRECTION ( 'NONE',  ( 0.000000000000000000, 1.000000000000000000, 0.000000000000000000 ) ) ;
#11333 = EDGE_CURVE ( 'NONE', #7550, #2200, #8027, .T. ) ;
#11334 = LINE ( 'NONE', #6176, #233 ) ;
#11336 = EDGE_CURVE ( 'NONE', #13099, #3963, #366, .T. ) ;
#11335 = ORIENTED_EDGE ( 'NONE', *, *, #7794, .T. ) ;
#11337 = LINE ( 'NONE', #284, #6930 ) ;
#11338 = ORIENTED_EDGE ( 'NONE', *, *, #12862, .F. ) ;
#11339 = CARTESIAN_POINT ( 'NONE',  ( 4.999999999999845457, -1.272547481429021854, -7.086597482644653390 ) ) ;
#11340 = DIRECTION ( 'NONE',  ( 0.000000000000000000, 1.000000000000000000, 0.000000000000000000 ) ) ;
#11341 = ORIENTED_EDGE ( 'NONE', *, *, #9020, .F. ) ;
#11342 = CARTESIAN_POINT ( 'NONE',  ( 0.5093500532425063732, 4.799145180956616130, -8.374999998634409692 ) ) ;
#11343 =( NAMED_UNIT ( * ) PLANE_ANGLE_UNIT ( ) SI_UNIT ( $, .RADIAN. ) );
#11344 = CARTESIAN_POINT ( 'NONE',  ( -4.209348295687703079, -3.401574460001763445, -5.312499997268816720 ) ) ;
#11345 = FACE_OUTER_BOUND ( 'NONE', #14797, .T. ) ;
#11346 = CARTESIAN_POINT ( 'NONE',  ( -3.401574460001764777, 4.209348295687701302, -3.562499997268815832 ) ) ;
#11347 = CARTESIAN_POINT ( 'NONE',  ( -5.000000000000004441, -7.530481206757679743E-15, -2.545263047592944972 ) ) ;
#11348 =( REPRESENTATION_RELATIONSHIP ('NONE','NONE', #4176, #4696 ) REPRESENTATION_RELATIONSHIP_WITH_TRANSFORMATION ( #1872 )SHAPE_REPRESENTATION_RELATIONSHIP( ) );
#11349 = ADVANCED_FACE ( 'NONE', ( #9384 ), #9311, .T. ) ;
#11350 = FACE_OUTER_BOUND ( 'NONE', #1808, .T. ) ;
#11351 = FACE_OUTER_BOUND ( 'NONE', #689, .T. ) ;
#11352 = EDGE_CURVE ( 'NONE', #9981, #1886, #10606, .T. ) ;
#11353 = EDGE_LOOP ( 'NONE', ( #14285, #8266, #179, #9586 ) ) ;
#11354 = DIRECTION ( 'NONE',  ( -0.000000000000000000, -0.000000000000000000, 1.000000000000000000 ) ) ;
#11355 = DIRECTION ( 'NONE',  ( -0.000000000000000000, 1.000000000000000000, 0.000000000000000000 ) ) ;
#11356 = CARTESIAN_POINT ( 'NONE',  ( 7.500000000000000888, 4.330127018922199866, -1.000000000000000888 ) ) ;
#11357 = ORIENTED_EDGE ( 'NONE', *, *, #12684, .T. ) ;
#11358 = EDGE_LOOP ( 'NONE', ( #4160, #7327, #1991, #13764 ) ) ;
#11359 = ORIENTED_EDGE ( 'NONE', *, *, #8676, .F. ) ;
#11360 = DIRECTION ( 'NONE',  ( -1.000000000000000000, 0.000000000000000000, 0.000000000000000000 ) ) ;
#11361 = CARTESIAN_POINT ( 'NONE',  ( -49.14213562373094391, -4.142135623730951899, -17.49999999999999645 ) ) ;
#11362 = CARTESIAN_POINT ( 'NONE',  ( -9.184850993605147944E-16, -27.37500000273118772, 5.000000000000000000 ) ) ;
#11363 = CARTESIAN_POINT ( 'NONE',  ( -5.000000000000000888, 6.123233995736767268E-16, -25.03750572909317285 ) ) ;
#11364 = CARTESIAN_POINT ( 'NONE',  ( -5.335963852939856977, -6.035591050534137025, -7.593821156097345870 ) ) ;
#11365 = FACE_OUTER_BOUND ( 'NONE', #3716, .T. ) ;
#11366 = CARTESIAN_POINT ( 'NONE',  ( -5.381735091635034607, 0.5711823568785950878, -5.562500000000000000 ) ) ;
#11367 = CYLINDRICAL_SURFACE ( 'NONE', #3951, 10.00000000000000000 ) ;
#11368 = EDGE_CURVE ( 'NONE', #580, #10196, #278, .T. ) ;
#11369 = DIRECTION ( 'NONE',  ( 0.000000000000000000, 1.000000000000000000, 0.000000000000000000 ) ) ;
#11370 = CARTESIAN_POINT ( 'NONE',  ( -1.846868145590737420, -23.75000000136559208, 4.458734124999999437 ) ) ;
#11371 = EDGE_CURVE ( 'NONE', #9071, #11683, #1954, .T. ) ;
#11372 = CARTESIAN_POINT ( 'NONE',  ( -4.276409079477644148, -1.261996585732578335, -5.062499998634406140 ) ) ;
#11373 = ORIENTED_EDGE ( 'NONE', *, *, #12452, .F. ) ;
#11374 = DIRECTION ( 'NONE',  ( 0.000000000000000000, 0.000000000000000000, 1.000000000000000000 ) ) ;
#11375 = ORIENTED_EDGE ( 'NONE', *, *, #14900, .T. ) ;
#11376 = VERTEX_POINT ( 'NONE', #2021 ) ;
#11377 = CARTESIAN_POINT ( 'NONE',  ( 1.846868145590735200, -29.50000000136559564, -4.458734125000000326 ) ) ;
#11378 = FACE_OUTER_BOUND ( 'NONE', #7618, .T. ) ;
#11379 = ORIENTED_EDGE ( 'NONE', *, *, #4253, .F. ) ;
#11380 = CARTESIAN_POINT ( 'NONE',  ( -3.535533905932737309, -28.62500000000000000, -3.535533905932738197 ) ) ;
#11381 = CARTESIAN_POINT ( 'NONE',  ( -21.01110699893060030, -1.230770033143087371E-15, 36.39230484541324273 ) ) ;
#11382 = CARTESIAN_POINT ( 'NONE',  ( -2.131511515620587272, -3.916244202832140253, -1.687499998634406362 ) ) ;
#11383 = DIRECTION ( 'NONE',  ( 0.000000000000000000, 0.8660254037844380415, -0.5000000000000012212 ) ) ;
#11384 = CARTESIAN_POINT ( 'NONE',  ( 3.535533905932736864, -30.12500000000000000, 3.535533905932738641 ) ) ;
#11385 = CARTESIAN_POINT ( 'NONE',  ( -2.500000000000000888, -7.216878364870333407, -7.063244554130006847 ) ) ;
#11386 = LINE ( 'NONE', #13722, #11545 ) ;
#11387 = CARTESIAN_POINT ( 'NONE',  ( 2.071067811865476394, -24.31250000273118772, 5.000000000000000000 ) ) ;
#11388 = EDGE_CURVE ( 'NONE', #15211, #15708, #11749, .T. ) ;
#11389 = CARTESIAN_POINT ( 'NONE',  ( -67.50000000000000000, 40.00000000000000000, 2.649999999999285816 ) ) ;
#11390 = CARTESIAN_POINT ( 'NONE',  ( -1.846868145590737420, -30.75000000136559919, 4.458734124999997661 ) ) ;
#11391 = CARTESIAN_POINT ( 'NONE',  ( 2.602085213965210642E-15, 8.660254037844392627, -1.000000000000000888 ) ) ;
#11392 = ORIENTED_EDGE ( 'NONE', *, *, #6933, .F. ) ;
#11393 = ORIENTED_EDGE ( 'NONE', *, *, #7878, .F. ) ;
#11394 = ORIENTED_EDGE ( 'NONE', *, *, #14228, .F. ) ;
#11395 = DIRECTION ( 'NONE',  ( 0.000000000000000000, 1.000000000000000000, 0.000000000000000000 ) ) ;
#11396 =( BOUNDED_CURVE ( )  B_SPLINE_CURVE ( 2, ( #11947, #13164, #2098 ),
 .UNSPECIFIED., .F., .F. ) 
 B_SPLINE_CURVE_WITH_KNOTS ( ( 3, 3 ),
 ( 0.2000000000000001776, 0.2045872658012772849 ),
 .UNSPECIFIED. ) 
 CURVE ( )  GEOMETRIC_REPRESENTATION_ITEM ( )  RATIONAL_B_SPLINE_CURVE ( ( 0.9999999999999990008, 0.9720652146169426189, 0.9646335149384808183 ) ) 
 REPRESENTATION_ITEM ( '' )  );
#11397 = ORIENTED_EDGE ( 'NONE', *, *, #9017, .T. ) ;
#11398 = CARTESIAN_POINT ( 'NONE',  ( -28.86751345948126612, 0.000000000000000000, -18.00000000000000355 ) ) ;
#11399 = VECTOR ( 'NONE', #3110, 1000.000000000000000 ) ;
#11400 = ADVANCED_FACE ( 'NONE', ( #2096 ), #896, .F. ) ;
#11401 = CARTESIAN_POINT ( 'NONE',  ( 4.209348295687701302, 3.401574460001766109, -1.812499997268814278 ) ) ;
#11402 = DIRECTION ( 'NONE',  ( 0.000000000000000000, 1.000000000000000000, 0.000000000000000000 ) ) ;
#11403 = CARTESIAN_POINT ( 'NONE',  ( 0.5711823568785988625, 5.381735091635026613, -6.687499997268816720 ) ) ;
#11404 = CARTESIAN_POINT ( 'NONE',  ( -35.00000000000000000, 55.00000000000000711, 0.000000000000000000 ) ) ;
#11405 = CARTESIAN_POINT ( 'NONE',  ( 3.033343224707661712, -3.753672977998669946, -4.749999998634407028 ) ) ;
#11406 = CARTESIAN_POINT ( 'NONE',  ( -91.33974596215558961, -105.7735026918962404, 7.500000000000001776 ) ) ;
#11407 = ORIENTED_EDGE ( 'NONE', *, *, #3684, .F. ) ;
#11408 = CARTESIAN_POINT ( 'NONE',  ( -7.500000000000003553, -2.886751345948131320, -7.198902722707431145 ) ) ;
#11409 = ORIENTED_EDGE ( 'NONE', *, *, #2659, .T. ) ;
#11410 = CARTESIAN_POINT ( 'NONE',  ( -55.00000000000000000, 0.000000000000000000, 19.99999999999999289 ) ) ;
#11411 = CARTESIAN_POINT ( 'NONE',  ( -3.152801135295367096, -31.06250000136559564, -3.152801135295367541 ) ) ;
#11412 = ORIENTED_EDGE ( 'NONE', *, *, #383, .F. ) ;
#11413 = ITEM_DEFINED_TRANSFORMATION ( 'NONE', 'NONE', #2947,  #3223 ) ;
#11414 = CARTESIAN_POINT ( 'NONE',  ( -3.916244202832140253, 2.131511515620587272, -5.187499998634406140 ) ) ;
#11415 = CIRCLE ( 'NONE', #13996, 2.649999999999985700 ) ;
#11416 = ADVANCED_FACE ( 'NONE', ( #14392 ), #3320, .T. ) ;
#11417 = AXIS2_PLACEMENT_3D ( 'NONE', #11752, #551, #14436 ) ;
#11418 = EDGE_CURVE ( 'NONE', #3993, #2783, #11707, .T. ) ;
#11419 = DIRECTION ( 'NONE',  ( 0.000000000000000000, 0.000000000000000000, 1.000000000000000000 ) ) ;
#11420 = DIRECTION ( 'NONE',  ( 0.000000000000000000, 0.000000000000000000, -1.000000000000000000 ) ) ;
#11421 = PRODUCT_DEFINITION_CONTEXT ( 'detailed design', #14873, 'design' ) ;
#11422 = CARTESIAN_POINT ( 'NONE',  ( -1.415196051561583790, 4.795541693661363958, -3.624999997268816276 ) ) ;
#11423 = CARTESIAN_POINT ( 'NONE',  ( 0.000000000000000000, -13.00000000000000178, -1.500000000000000000 ) ) ;
#11424 = CARTESIAN_POINT ( 'NONE',  ( -1.654942507329426382, 4.210624982170731556, -0.3352054413388214082 ) ) ;
#11425 = CARTESIAN_POINT ( 'NONE',  ( 4.458734124999999437, -23.62500000136559564, -1.846868145590734978 ) ) ;
#11426 = VERTEX_POINT ( 'NONE', #10983 ) ;
#11427 = DIRECTION ( 'NONE',  ( -1.000000000000000000, 0.000000000000000000, 0.000000000000000000 ) ) ;
#11428 = CARTESIAN_POINT ( 'NONE',  ( 7.500000000000000000, -5.204170427930421283E-15, -6.991905250253757309 ) ) ;
#11429 = CIRCLE ( 'NONE', #4467, 31.99999999999999289 ) ;
#11430 = DIRECTION ( 'NONE',  ( 0.000000000000000000, 0.000000000000000000, 1.000000000000000000 ) ) ;
#11431 = VERTEX_POINT ( 'NONE', #1116 ) ;
#11432 = ORIENTED_EDGE ( 'NONE', *, *, #6597, .F. ) ;
#11433 = EDGE_LOOP ( 'NONE', ( #8993, #14555, #8864, #10344 ) ) ;
#11434 = CARTESIAN_POINT ( 'NONE',  ( -5.000000000000091482, -0.7223674278660691117, -0.5217993655171538903 ) ) ;
#11435 = DIRECTION ( 'NONE',  ( 2.775557561562896479E-15, -1.000000000000000000, -0.000000000000000000 ) ) ;
#11436 = DIRECTION ( 'NONE',  ( 0.8191520442889875797, 0.000000000000000000, 0.5735764363510522656 ) ) ;
#11437 = EDGE_CURVE ( 'NONE', #7472, #482, #15638, .T. ) ;
#11438 = APPLICATION_CONTEXT ( 'automotive_design' ) ;
#11439 = CARTESIAN_POINT ( 'NONE',  ( -7.263825692932306843, -4.945657111639584436, -7.907570769506049757 ) ) ;
#11440 = CARTESIAN_POINT ( 'NONE',  ( -7.847095227763516867, -4.129731495738497848, -7.493596212620241559 ) ) ;
#11441 = CARTESIAN_POINT ( 'NONE',  ( -41.99999999999978684, -9.000000000000001776, -3.500000000000001776 ) ) ;
#11442 = CARTESIAN_POINT ( 'NONE',  ( -2.390265326283148806, -4.391654775818394363, -5.375000000000000888 ) ) ;
#11443 = DIRECTION ( 'NONE',  ( -0.8660254037844402619, 0.4999999999999973910, 0.000000000000000000 ) ) ;
#11444 = CARTESIAN_POINT ( 'NONE',  ( 3.535533905932736864, -29.12500000000000000, 3.535533905932738641 ) ) ;
#11445 = CARTESIAN_POINT ( 'NONE',  ( 4.458734124999999437, -23.43750000136559564, 0.000000000000000000 ) ) ;
#11446 = CARTESIAN_POINT ( 'NONE',  ( 0.5093500532425063732, 4.799145180956616130, -5.374999998634406140 ) ) ;
#11447 = ORIENTED_EDGE ( 'NONE', *, *, #9598, .T. ) ;
#11448 = UNCERTAINTY_MEASURE_WITH_UNIT (LENGTH_MEASURE( 1.000000000000000082E-05 ), #14334, 'distance_accuracy_value', 'NONE');
#11449 = CARTESIAN_POINT ( 'NONE',  ( 2.500000000000000000, 7.216878364870322748, -7.063244554130002406 ) ) ;
#11450 = EDGE_LOOP ( 'NONE', ( #13368, #15475, #9962 ) ) ;
#11451 = ORIENTED_EDGE ( 'NONE', *, *, #15220, .T. ) ;
#11452 = CARTESIAN_POINT ( 'NONE',  ( -4.458734124999999437, -21.93750000136559208, -5.460374474430324690E-16 ) ) ;
#11453 = CARTESIAN_POINT ( 'NONE',  ( -28.86751345948129455, 88.59290746114278647, 49.99999999999999289 ) ) ;
#11454 = ORIENTED_EDGE ( 'NONE', *, *, #7399, .T. ) ;
#11455 = CARTESIAN_POINT ( 'NONE',  ( -0.02448733951239248641, -4.877042772274742255, -3.751161874094027571 ) ) ;
#11456 = ADVANCED_FACE ( 'NONE', ( #971 ), #7120, .T. ) ;
#11457 = ADVANCED_FACE ( 'NONE', ( #6225 ), #13231, .T. ) ;
#11458 = ADVANCED_FACE ( 'NONE', ( #9924 ), #5899, .T. ) ;
#11459 = FACE_OUTER_BOUND ( 'NONE', #4390, .T. ) ;
#11460 = CARTESIAN_POINT ( 'NONE',  ( 3.916244202832140253, -2.131511515620588160, -1.437499998634406140 ) ) ;
#11461 = CARTESIAN_POINT ( 'NONE',  ( 2.500000000000000000, 2.357898499370433054, -1.951563910473907981E-15 ) ) ;
#11462 = CARTESIAN_POINT ( 'NONE',  ( -3.535533905932737309, -30.62500000000000000, -3.535533905932738197 ) ) ;
#11463 = CARTESIAN_POINT ( 'NONE',  ( -0.6937372685066653943, 4.453844082567723461, -3.610536846335889116 ) ) ;
#11464 = LINE ( 'NONE', #13801, #3545 ) ;
#11465 = CARTESIAN_POINT ( 'NONE',  ( 3.061616997868383141E-16, -24.87500000273118417, -5.000000000000000000 ) ) ;
#11466 = CARTESIAN_POINT ( 'NONE',  ( 1.415196051561583790, -4.795541693661363958, -3.250000000000002665 ) ) ;
#11467 = AXIS2_PLACEMENT_3D ( 'NONE', #7231, #9712, #2195 ) ;
#11468 = CARTESIAN_POINT ( 'NONE',  ( -3.152801135295367096, -27.06250000136559564, -3.152801135295367541 ) ) ;
#11469 = LINE ( 'NONE', #1613, #2196 ) ;
#11470 = VERTEX_POINT ( 'NONE', #4921 ) ;
#11471 = ORIENTED_EDGE ( 'NONE', *, *, #4162, .T. ) ;
#11472 = ORIENTED_EDGE ( 'NONE', *, *, #7153, .T. ) ;
#11473 = CARTESIAN_POINT ( 'NONE',  ( -44.15702331412045822, -3.242827243955582084, 21.01093009162843117 ) ) ;
#11474 = VERTEX_POINT ( 'NONE', #15923 ) ;
#11475 = DIRECTION ( 'NONE',  ( 0.000000000000000000, 0.000000000000000000, -1.000000000000000000 ) ) ;
#11476 = COLOUR_RGB ( '', 0.66274510, 0.83137255, 0.94901961) ;
#11477 = EDGE_CURVE ( 'NONE', #8470, #12690, #2981, .T. ) ;
#11478 = COLOUR_RGB ( '', 0.08235294, 0.09019608, 0.10196078) ;
#11479 = CARTESIAN_POINT ( 'NONE',  ( 57.73502691896258199, 0.000000000000000000, 2.081668171172168513E-14 ) ) ;
#11480 = MECHANICAL_DESIGN_GEOMETRIC_PRESENTATION_REPRESENTATION (  '', ( #1420 ), #9937 ) ;
#11481 = CARTESIAN_POINT ( 'NONE',  ( 4.458734125000000326, -31.62500000136559564, -1.846868145590734978 ) ) ;
#11482 = CONTEXT_DEPENDENT_SHAPE_REPRESENTATION ( #8581, #8106 ) ;
#11483 = CARTESIAN_POINT ( 'NONE',  ( -3.401574460001765221, 4.209348295687701302, -7.562499997268815832 ) ) ;
#11484 = PLANE ( 'NONE',  #7667 ) ;
#11485 = ORIENTED_EDGE ( 'NONE', *, *, #36, .T. ) ;
#11486 =( BOUNDED_CURVE ( )  B_SPLINE_CURVE ( 2, ( #10316, #450, #12464, #3909, #2854, #8855, #1403, #299, #15241 ),
 .UNSPECIFIED., .F., .F. ) 
 B_SPLINE_CURVE_WITH_KNOTS ( ( 3, 2, 2, 2, 3 ),
 ( 0.9545872658012772849, 0.9625000000000000222, 0.9749999999999999778, 0.9875000000000000444, 1.000000000000000000 ),
 .UNSPECIFIED. ) 
 CURVE ( )  GEOMETRIC_REPRESENTATION_ITEM ( )  RATIONAL_B_SPLINE_CURVE ( ( 0.9646335149384808183, 0.9518143178943441196, 1.000000000000000000, 0.9238795325112867385, 1.000000000000000000, 0.9238795325112867385, 1.000000000000000000, 0.9238795325112867385, 1.000000000000000000 ) ) 
 REPRESENTATION_ITEM ( '' )  );
#11487 = VECTOR ( 'NONE', #1192, 1000.000000000000000 ) ;
#11488 = ORIENTED_EDGE ( 'NONE', *, *, #979, .F. ) ;
#11489 = DIRECTION ( 'NONE',  ( -0.000000000000000000, -1.000000000000000000, -0.000000000000000000 ) ) ;
#11490 = DIRECTION ( 'NONE',  ( 0.000000000000000000, 1.000000000000000000, 0.000000000000000000 ) ) ;
#11491 = VECTOR ( 'NONE', #10116, 1000.000000000000114 ) ;
#11492 = ORIENTED_EDGE ( 'NONE', *, *, #4999, .T. ) ;
#11493 = CARTESIAN_POINT ( 'NONE',  ( 0.5093500532425063732, 4.799145180956616130, -7.374999998634407916 ) ) ;
#11494 = CARTESIAN_POINT ( 'NONE',  ( -17.99999999999979394, -9.000000000000001776, -1.500000000000000888 ) ) ;
#11495 = AXIS2_PLACEMENT_3D ( 'NONE', #6031, #7253, #12153 ) ;
#11496 = CARTESIAN_POINT ( 'NONE',  ( 3.061616997868383141E-16, -28.87500000273118772, -5.000000000000000000 ) ) ;
#11497 = CARTESIAN_POINT ( 'NONE',  ( 30.02221399786054334, 0.000000000000000000, 16.00000000000000355 ) ) ;
#11498 = CIRCLE ( 'NONE', #14870, 75.00000000000004263 ) ;
#11499 = CARTESIAN_POINT ( 'NONE',  ( -4.209348295687703967, -3.401574460001763001, -2.312499997268814500 ) ) ;
#11500 = SPHERICAL_SURFACE ( 'NONE', #7078, 10.00000000000000000 ) ;
#11501 = CARTESIAN_POINT ( 'NONE',  ( 3.152801135295366208, -21.81250000136559208, 3.152801135295367985 ) ) ;
#11502 = ORIENTED_EDGE ( 'NONE', *, *, #8327, .T. ) ;
#11503 = CARTESIAN_POINT ( 'NONE',  ( 19.99999999999956657, -8.786575603324269439E-13, 0.000000000000000000 ) ) ;
#11504 = DIRECTION ( 'NONE',  ( -0.9999824063907751803, -0.005931855436079011210, -0.000000000000000000 ) ) ;
#11505 = CARTESIAN_POINT ( 'NONE',  ( -5.000000000000000888, -26.56250000273118772, 2.071067811865474617 ) ) ;
#11506 = ADVANCED_FACE ( 'NONE', ( #3627 ), #7204, .F. ) ;
#11507 = ORIENTED_EDGE ( 'NONE', *, *, #9553, .F. ) ;
#11508 = CARTESIAN_POINT ( 'NONE',  ( -4.000000000000000000, -1.680117682357936904, -3.316611593218794951 ) ) ;
#11509 = ORIENTED_EDGE ( 'NONE', *, *, #6306, .T. ) ;
#11510 = VECTOR ( 'NONE', #4405, 1000.000000000000000 ) ;
#11511 = ORIENTED_EDGE ( 'NONE', *, *, #780, .F. ) ;
#11512 = CARTESIAN_POINT ( 'NONE',  ( -21.01110699893060030, -3.000000000000001332, 33.74230484541325126 ) ) ;
#11513 = CARTESIAN_POINT ( 'NONE',  ( 0.000000000000000000, 0.000000000000000000, -4.000000000000000000 ) ) ;
#11514 = AXIS2_PLACEMENT_3D ( 'NONE', #12442, #11008, #14725 ) ;
#11515 = DIRECTION ( 'NONE',  ( 0.000000000000000000, 0.000000000000000000, -1.000000000000000000 ) ) ;
#11516 = CLOSED_SHELL ( 'NONE', ( #1235, #6803, #14781, #3254, #3665, #9720, #1555, #364, #4932, #9789, #15030, #12248, #1933, #833, #7025, #3924, #10991, #4704, #3755, #13412, #956, #3279, #11400, #12324, #4545, #8197, #5880, #12011, #21, #2083 ) ) ;
#11517 = CARTESIAN_POINT ( 'NONE',  ( -6.765421556309547668E-13, 37.00000000000000000, 67.49999999999930367 ) ) ;
#11519 = CARTESIAN_POINT ( 'NONE',  ( 0.3483149870578527429, -8.861353789385033153, -7.493854785173817312 ) ) ;
#11518 = CIRCLE ( 'NONE', #1209, 5.000000000000000888 ) ;
#11520 = DIRECTION ( 'NONE',  ( 0.000000000000000000, 0.000000000000000000, -1.000000000000000000 ) ) ;
#11521 = CARTESIAN_POINT ( 'NONE',  ( 4.795541693661363958, 1.415196051561583790, -7.000000000000002665 ) ) ;
#11522 = PLANE ( 'NONE',  #14158 ) ;
#11523 = DIRECTION ( 'NONE',  ( 0.000000000000000000, 0.000000000000000000, 1.000000000000000000 ) ) ;
#11524 = CARTESIAN_POINT ( 'NONE',  ( 4.458734124999997661, -26.75000000136559564, 1.846868145590737864 ) ) ;
#11525 = CIRCLE ( 'NONE', #7928, 9.999999999999994671 ) ;
#11526 = CARTESIAN_POINT ( 'NONE',  ( 2.131511515620586383, 3.916244202832140253, -5.437499998634406140 ) ) ;
#11527 = ORIENTED_EDGE ( 'NONE', *, *, #13016, .T. ) ;
#11528 = CARTESIAN_POINT ( 'NONE',  ( -4.336808689942017736E-16, 9.147862274876558786, -8.047472243342932430 ) ) ;
#11529 = ADVANCED_FACE ( 'NONE', ( #5 ), #3460, .T. ) ;
#11530 = VERTEX_POINT ( 'NONE', #14621 ) ;
#11531 = ORIENTED_EDGE ( 'NONE', *, *, #15882, .T. ) ;
#11532 = EDGE_CURVE ( 'NONE', #10685, #9400, #14778, .T. ) ;
#11533 = CARTESIAN_POINT ( 'NONE',  ( -1.846868145590734756, -22.12500000136559564, -4.458734125000000326 ) ) ;
#11534 = FACE_OUTER_BOUND ( 'NONE', #9033, .T. ) ;
#11535 = CIRCLE ( 'NONE', #9234, 5.000000000000000888 ) ;
#11536 = EDGE_LOOP ( 'NONE', ( #13078, #2857, #3734, #9126 ) ) ;
#11537 = CARTESIAN_POINT ( 'NONE',  ( 0.000000000000000000, 5.051668046482832750E-16, -4.000000000000000000 ) ) ;
#11538 = VECTOR ( 'NONE', #14108, 1000.000000000000000 ) ;
#11539 = CARTESIAN_POINT ( 'NONE',  ( 7.500000000000000000, 3.948247735265757452, -7.349893093596098659 ) ) ;
#11540 = CARTESIAN_POINT ( 'NONE',  ( 0.5093500532425063732, 4.799145180956616130, -1.124999998634405918 ) ) ;
#11541 = CARTESIAN_POINT ( 'NONE',  ( 3.528469415195318426, 2.738956135389102098, -0.3789984458506761023 ) ) ;
#11542 = CARTESIAN_POINT ( 'NONE',  ( -5.000000000000000888, -26.56249999999999645, -2.071067811865475949 ) ) ;
#11543 = CARTESIAN_POINT ( 'NONE',  ( -2.131511515620587272, -3.916244202832140253, -3.687499998634407916 ) ) ;
#11544 = CARTESIAN_POINT ( 'NONE',  ( -2.344047193898593395, -3.265465875126480455, -1.054683074273691752E-14 ) ) ;
#11545 = VECTOR ( 'NONE', #2738, 1000.000000000000000 ) ;
#11546 = AXIS2_PLACEMENT_3D ( 'NONE', #6656, #9082, #669 ) ;
#11547 = CARTESIAN_POINT ( 'NONE',  ( -9.184850993605147944E-16, -30.37500000273118772, 5.000000000000000000 ) ) ;
#11548 = CARTESIAN_POINT ( 'NONE',  ( 2.071067811865476394, -25.31250000273118062, 5.000000000000000000 ) ) ;
#11549 = CYLINDRICAL_SURFACE ( 'NONE', #3685, 5.000000000000000888 ) ;
#11550 = CARTESIAN_POINT ( 'NONE',  ( 3.152801135295367541, -27.31250000136559564, -3.152801135295367541 ) ) ;
#11551 = EDGE_CURVE ( 'NONE', #14039, #6759, #10990, .T. ) ;
#11552 = DIRECTION ( 'NONE',  ( 0.000000000000000000, 0.000000000000000000, 1.000000000000000000 ) ) ;
#11553 = ORIENTED_EDGE ( 'NONE', *, *, #12032, .F. ) ;
#11554 = ORIENTED_EDGE ( 'NONE', *, *, #14672, .T. ) ;
#11555 = EDGE_CURVE ( 'NONE', #14284, #13587, #923, .T. ) ;
#11556 = AXIS2_PLACEMENT_3D ( 'NONE', #15379, #4302, #10298 ) ;
#11557 = EDGE_LOOP ( 'NONE', ( #5829, #12421, #2565, #13390 ) ) ;
#11558 = CARTESIAN_POINT ( 'NONE',  ( 7.808623696107322765, 4.508310992947620832, -7.999704684617482187 ) ) ;
#11559 = EDGE_LOOP ( 'NONE', ( #7159, #2986 ) ) ;
#11560 = CARTESIAN_POINT ( 'NONE',  ( 47.32050807568879947, -37.00000000000000711, -41.96152422706630603 ) ) ;
#11561 = LINE ( 'NONE', #515, #7827 ) ;
#11562 = CARTESIAN_POINT ( 'NONE',  ( 4.458734125000000326, -29.62500000136559208, -1.846868145590734978 ) ) ;
#11563 = AXIS2_PLACEMENT_3D ( 'NONE', #15796, #14567, #13420 ) ;
#11564 = CARTESIAN_POINT ( 'NONE',  ( -4.391654775818395251, 2.390265326283148806, -6.499999997268815832 ) ) ;
#11565 = ITEM_DEFINED_TRANSFORMATION ( 'NONE', 'NONE', #5276,  #3223 ) ;
#11566 = CARTESIAN_POINT ( 'NONE',  ( -4.391654775818395251, 2.390265326283148806, -7.499999997268816720 ) ) ;
#11567 = DIRECTION ( 'NONE',  ( -0.000000000000000000, 1.000000000000000000, -0.000000000000000000 ) ) ;
#11568 = AXIS2_PLACEMENT_3D ( 'NONE', #15500, #14201, #5631 ) ;
#11569 = EDGE_LOOP ( 'NONE', ( #10933, #3994 ) ) ;
#11570 = EDGE_CURVE ( 'NONE', #6761, #4915, #2400, .T. ) ;
#11571 =( NAMED_UNIT ( * ) PLANE_ANGLE_UNIT ( ) SI_UNIT ( $, .RADIAN. ) );
#11572 = VERTEX_POINT ( 'NONE', #2331 ) ;
#11573 = DIRECTION ( 'NONE',  ( 1.982541115402065110E-16, -1.000000000000000000, -0.000000000000000000 ) ) ;
#11574 = CARTESIAN_POINT ( 'NONE',  ( -3.152801135295367096, -30.06250000136559564, -3.152801135295367541 ) ) ;
#11575 = COLOUR_RGB ( '', 0.09019608, 0.27058824, 0.51372549) ;
#11576 = VECTOR ( 'NONE', #12046, 1000.000000000000000 ) ;
#11577 = VERTEX_POINT ( 'NONE', #8647 ) ;
#11578 = AXIS2_PLACEMENT_3D ( 'NONE', #10741, #884, #8015 ) ;
#11579 = CIRCLE ( 'NONE', #4621, 28.00000000000000355 ) ;
#11580 = DIRECTION ( 'NONE',  ( 0.000000000000000000, 0.000000000000000000, 1.000000000000000000 ) ) ;
#11581 = CARTESIAN_POINT ( 'NONE',  ( 4.999999999999845457, -1.272547481429021854, -7.961597479913462116 ) ) ;
#11582 =( BOUNDED_CURVE ( )  B_SPLINE_CURVE ( 2, ( #293, #5206, #10139, #15065, #7734 ),
 .UNSPECIFIED., .F., .F. ) 
 B_SPLINE_CURVE_WITH_KNOTS ( ( 3, 2, 3 ),
 ( 0.9749999999999998668, 0.9875000000000000444, 1.000000000000000000 ),
 .UNSPECIFIED. ) 
 CURVE ( )  GEOMETRIC_REPRESENTATION_ITEM ( )  RATIONAL_B_SPLINE_CURVE ( ( 1.000000000000000666, 0.9238795325112860723, 1.000000000000000000, 0.9238795325112867385, 1.000000000000000000 ) ) 
 REPRESENTATION_ITEM ( '' )  );
#11583 = CARTESIAN_POINT ( 'NONE',  ( -3.916244202832140253, 2.131511515620587272, 0.8125000013655924169 ) ) ;
#11584 = LINE ( 'NONE', #7967, #7598 ) ;
#11585 = DIRECTION ( 'NONE',  ( 1.000000000000000000, 0.000000000000000000, 0.000000000000000000 ) ) ;
#11586 = CARTESIAN_POINT ( 'NONE',  ( -1.846868145590734756, -23.37500000136559564, -4.458734124999999437 ) ) ;
#11587 = VERTEX_POINT ( 'NONE', #6141 ) ;
#11588 = CARTESIAN_POINT ( 'NONE',  ( 4.575072720889181710, -0.1979831123187004716, -0.2975372840247698103 ) ) ;
#11589 = CARTESIAN_POINT ( 'NONE',  ( -4.204015924366189871, 1.626724848190922446, -3.610627190413390419 ) ) ;
#11590 = EDGE_CURVE ( 'NONE', #1523, #15294, #13307, .T. ) ;
#11591 = CARTESIAN_POINT ( 'NONE',  ( 0.000000000000000000, 0.000000000000000000, 3.469446951953614189E-15 ) ) ;
#11592 = EDGE_LOOP ( 'NONE', ( #672, #3414, #3604, #12811 ) ) ;
#11593 = CARTESIAN_POINT ( 'NONE',  ( -4.211405944401398038, -2.460460786169389902, -3.751298493805494072 ) ) ;
#11594 = ORIENTED_EDGE ( 'NONE', *, *, #12143, .F. ) ;
#11595 = ORIENTED_EDGE ( 'NONE', *, *, #15753, .F. ) ;
#11596 = CARTESIAN_POINT ( 'NONE',  ( -2.390265326283148806, -4.391654775818394363, -0.3750000000000003331 ) ) ;
#11597 = CARTESIAN_POINT ( 'NONE',  ( -3.455068668934486276, 2.624017327439035707, -3.316620875263955437 ) ) ;
#11598 = CARTESIAN_POINT ( 'NONE',  ( -6.293430271071540183, 5.026740376715094882, -0.4524126574264508149 ) ) ;
#11599 = EDGE_CURVE ( 'NONE', #946, #4042, #2250, .T. ) ;
#11600 = CARTESIAN_POINT ( 'NONE',  ( -5.000000000000004441, -1.011557177027151181E-15, -5.545263047592944972 ) ) ;
#11601 = CARTESIAN_POINT ( 'NONE',  ( 11.45098066423670247, -3.000000000000000000, 1.122567565269603304E-11 ) ) ;
#11602 = CARTESIAN_POINT ( 'NONE',  ( 4.420982230657666712, -0.5789871446316176007, -0.3789984458506777676 ) ) ;
#11603 = CYLINDRICAL_SURFACE ( 'NONE', #11936, 5.000000000000000000 ) ;
#11604 = CARTESIAN_POINT ( 'NONE',  ( 3.535533905932736864, -25.25000000273118417, 3.535533905932738641 ) ) ;
#11605 = CARTESIAN_POINT ( 'NONE',  ( 1.846868145590736310, -21.62500000136559564, 4.458734124999999437 ) ) ;
#11606 = CARTESIAN_POINT ( 'NONE',  ( 3.916244202832140253, -2.131511515620588160, -4.687499998634405252 ) ) ;
#11607 = ORIENTED_EDGE ( 'NONE', *, *, #5242, .F. ) ;
#11608 = CARTESIAN_POINT ( 'NONE',  ( 2.602085213965210642E-15, 8.660254037844392627, -7.422398894150035176 ) ) ;
#11609 = ORIENTED_EDGE ( 'NONE', *, *, #5753, .T. ) ;
#11610 = ORIENTED_EDGE ( 'NONE', *, *, #10670, .T. ) ;
#11611 = CARTESIAN_POINT ( 'NONE',  ( -8.190561711645485556E-16, -21.68750000136559208, 4.458734124999999437 ) ) ;
#11612 = DIRECTION ( 'NONE',  ( 0.000000000000000000, 1.000000000000000000, 0.000000000000000000 ) ) ;
#11613 = EDGE_LOOP ( 'NONE', ( #378, #15365 ) ) ;
#11614 = CARTESIAN_POINT ( 'NONE',  ( -4.795541693661363958, -1.415196051561583790, -6.500000000000002665 ) ) ;
#11615 = DIRECTION ( 'NONE',  ( 0.000000000000000000, 0.000000000000000000, -1.000000000000000000 ) ) ;
#11616 = EDGE_CURVE ( 'NONE', #10728, #865, #1044, .T. ) ;
#11617 = CARTESIAN_POINT ( 'NONE',  ( 3.033343224707661712, -3.753672977998669502, -4.499999998634407028 ) ) ;
#11618 = FACE_OUTER_BOUND ( 'NONE', #12878, .T. ) ;
#11619 = EDGE_CURVE ( 'NONE', #2121, #7238, #10901, .T. ) ;
#11620 = CARTESIAN_POINT ( 'NONE',  ( 2.071067811865475505, -25.81250000000000000, -5.000000000000000888 ) ) ;
#11621 = CARTESIAN_POINT ( 'NONE',  ( -0.5093500532425060401, -4.799145180956616130, -5.624999998634406140 ) ) ;
#11622 = CARTESIAN_POINT ( 'NONE',  ( -44.32078660371288237, -3.761076017575719188, -20.42441216671174686 ) ) ;
#11623 = CARTESIAN_POINT ( 'NONE',  ( -28.86751345948126257, 0.000000000000000000, -50.00000000000000711 ) ) ;
#11624 = CARTESIAN_POINT ( 'NONE',  ( 2.071067811865475505, -23.93750000273119483, -5.000000000000000888 ) ) ;
#11625 = CARTESIAN_POINT ( 'NONE',  ( -21.01110699893041911, -3.000000000000000000, -39.04230484541333368 ) ) ;
#11626 = CARTESIAN_POINT ( 'NONE',  ( -4.458734125000000326, -25.87500000136559564, 1.846868145590734089 ) ) ;
#11627 = CARTESIAN_POINT ( 'NONE',  ( 1.015826369459312373, -8.073766409986486536, -7.642786413609471197 ) ) ;
#11628 = EDGE_LOOP ( 'NONE', ( #6403, #7655 ) ) ;
#11629 = VERTEX_POINT ( 'NONE', #5325 ) ;
#11630 = DIRECTION ( 'NONE',  ( -0.000000000000000000, 1.000000000000000000, -0.000000000000000000 ) ) ;
#11631 = ORIENTED_EDGE ( 'NONE', *, *, #14991, .T. ) ;
#11632 = CARTESIAN_POINT ( 'NONE',  ( 5.000000000000000000, -29.18750000273119127, 2.071067811865478614 ) ) ;
#11633 = ORIENTED_EDGE ( 'NONE', *, *, #3128, .F. ) ;
#11634 = FACE_OUTER_BOUND ( 'NONE', #7842, .T. ) ;
#11635 = CARTESIAN_POINT ( 'NONE',  ( 7.897836333153806621, 1.530409084195002656, -7.633857274177626273 ) ) ;
#11636 = EDGE_CURVE ( 'NONE', #9335, #2497, #12735, .T. ) ;
#11637 = CARTESIAN_POINT ( 'NONE',  ( -4.458734125000001214, -28.12500000136559564, 1.846868145590734089 ) ) ;
#11638 = PLANE ( 'NONE',  #1855 ) ;
#11639 = B_SPLINE_CURVE_WITH_KNOTS ( 'NONE', 3,
 ( #2448, #1404, #12389, #1247, #8939, #5210, #11424, #12550, #10069, #3838, #14998, #3911, #371, #5139, #4966, #8781, #4072, #14830, #1572, #5288 ),
 .UNSPECIFIED., .F., .F.,
 ( 4, 2, 2, 2, 2, 2, 2, 2, 2, 4 ),
 ( 0.000000000000000000, 0.0009685699525029332598, 0.001937139905005866520, 0.002421424881257333312, 0.002905709857508799888, 0.003874279810011731304, 0.004842849762514664022, 0.005811419715017596306, 0.006779989667520527723, 0.007748559620023459139 ),
 .UNSPECIFIED. ) ;
#11640 = LINE ( 'NONE', #9391, #13369 ) ;
#11641 = DIRECTION ( 'NONE',  ( 1.000000000000000000, -1.387778780781446464E-15, 0.000000000000000000 ) ) ;
#11642 = CARTESIAN_POINT ( 'NONE',  ( -2.131511515620587272, -3.916244202832140253, 0.06250000136559172303 ) ) ;
#11643 = ORIENTED_EDGE ( 'NONE', *, *, #12323, .T. ) ;
#11644 = VERTEX_POINT ( 'NONE', #253 ) ;
#11645 = CARTESIAN_POINT ( 'NONE',  ( -21.01110699893060030, -3.000000000000000000, 36.39230484541324273 ) ) ;
#11646 = VERTEX_POINT ( 'NONE', #7769 ) ;
#11647 = CARTESIAN_POINT ( 'NONE',  ( 4.795541693661363958, 1.415196051561583790, -5.000000000000000888 ) ) ;
#11648 = PRODUCT_DEFINITION_SHAPE ( 'NONE', 'NONE',  #16001 ) ;
#11649 = EDGE_CURVE ( 'NONE', #3229, #11234, #684, .T. ) ;
#11650 = EDGE_CURVE ( 'NONE', #13261, #2513, #1188, .T. ) ;
#11651 = EDGE_CURVE ( 'NONE', #4563, #3351, #3869, .T. ) ;
#11652 = EDGE_CURVE ( 'NONE', #2292, #13118, #8888, .T. ) ;
#11653 = CYLINDRICAL_SURFACE ( 'NONE', #7725, 57.99999999999999289 ) ;
#11654 = FACE_OUTER_BOUND ( 'NONE', #2675, .T. ) ;
#11655 = CARTESIAN_POINT ( 'NONE',  ( 1.261996585732578113, -4.276409079477644148, 1.187500001365592750 ) ) ;
#11656 = DIRECTION ( 'NONE',  ( 0.000000000000000000, 0.000000000000000000, -1.000000000000000000 ) ) ;
#11657 =( LENGTH_UNIT ( ) NAMED_UNIT ( * ) SI_UNIT ( .MILLI., .METRE. ) );
#11658 = CYLINDRICAL_SURFACE ( 'NONE', #5031, 4.250000000000000000 ) ;
#11659 = EDGE_LOOP ( 'NONE', ( #4261, #12475, #7660, #5729 ) ) ;
#11660 = CARTESIAN_POINT ( 'NONE',  ( 19.99999999999956657, -8.786575603324269439E-13, -4.500000000000000000 ) ) ;
#11661 = CARTESIAN_POINT ( 'NONE',  ( 2.500000000000000000, -1.178949249685218303, -2.041999999999998039 ) ) ;
#11662 = LINE ( 'NONE', #457, #8654 ) ;
#11663 = ORIENTED_EDGE ( 'NONE', *, *, #521, .F. ) ;
#11664 = FACE_OUTER_BOUND ( 'NONE', #8351, .T. ) ;
#11665 = ORIENTED_EDGE ( 'NONE', *, *, #4427, .T. ) ;
#11666 = ORIENTED_EDGE ( 'NONE', *, *, #12683, .T. ) ;
#11667 = CARTESIAN_POINT ( 'NONE',  ( -2.071067811865489272, -30.68749999999999645, -4.999999999999985789 ) ) ;
#11668 = FACE_OUTER_BOUND ( 'NONE', #15919, .T. ) ;
#11669 = AXIS2_PLACEMENT_3D ( 'NONE', #8872, #15172, #4090 ) ;
#11670 = CARTESIAN_POINT ( 'NONE',  ( 0.000000000000000000, -11.00000000000000178, 0.000000000000000000 ) ) ;
#11671 = EDGE_CURVE ( 'NONE', #349, #13499, #15394, .T. ) ;
#11672 = CARTESIAN_POINT ( 'NONE',  ( 5.000000000000000000, -26.12500000273118417, 0.000000000000000000 ) ) ;
#11673 = DIRECTION ( 'NONE',  ( 0.000000000000000000, -1.000000000000000000, 0.000000000000000000 ) ) ;
#11674 = CARTESIAN_POINT ( 'NONE',  ( 5.000000000000004441, 0.000000000000000000, 0.000000000000000000 ) ) ;
#11675 = AXIS2_PLACEMENT_3D ( 'NONE', #14546, #11077, #14630 ) ;
#11676 = DIRECTION ( 'NONE',  ( 1.000000000000000000, -0.000000000000000000, -1.239088197126290570E-16 ) ) ;
#11677 = DIRECTION ( 'NONE',  ( -0.5000000000000004441, 0.000000000000000000, 0.8660254037844383745 ) ) ;
#11678 = AXIS2_PLACEMENT_3D ( 'NONE', #13963, #8977, #13889 ) ;
#11679 = DIRECTION ( 'NONE',  ( 0.000000000000000000, 0.000000000000000000, -1.000000000000000000 ) ) ;
#11680 = CARTESIAN_POINT ( 'NONE',  ( 1.846868145590736310, -23.62500000136559919, 4.458734124999999437 ) ) ;
#11681 = CARTESIAN_POINT ( 'NONE',  ( 1.261996585732578113, -4.276409079477644148, 0.4375000013655920839 ) ) ;
#11682 = ORIENTED_EDGE ( 'NONE', *, *, #9945, .F. ) ;
#11683 = VERTEX_POINT ( 'NONE', #4020 ) ;
#11684 = CARTESIAN_POINT ( 'NONE',  ( 35.00000000000000000, 37.00000000000000000, -5.999999999999991118 ) ) ;
#11685 = ORIENTED_EDGE ( 'NONE', *, *, #13427, .T. ) ;
#11686 = ORIENTED_EDGE ( 'NONE', *, *, #3443, .T. ) ;
#11687 = CARTESIAN_POINT ( 'NONE',  ( -3.152801135295367985, -31.06250000136559564, 3.152801135295367096 ) ) ;
#11688 = CARTESIAN_POINT ( 'NONE',  ( 14.41154273188013590, 88.59290746114278647, -60.96152422706631313 ) ) ;
#11689 = ORIENTED_EDGE ( 'NONE', *, *, #12701, .T. ) ;
#11690 = CARTESIAN_POINT ( 'NONE',  ( 5.000000000000004441, -2.247904837838113790E-16, -6.045263047592945860 ) ) ;
#11691 = CARTESIAN_POINT ( 'NONE',  ( -67.50000000000000000, 37.00000000000000000, -7.070249711157346244E-13 ) ) ;
#11692 = CARTESIAN_POINT ( 'NONE',  ( -4.276409079477644148, -1.261996585732578335, -5.812499998634406140 ) ) ;
#11693 = CARTESIAN_POINT ( 'NONE',  ( 5.000000000000002665, 1.275685995473128912E-14, -5.920263044861758139 ) ) ;
#11694 = CARTESIAN_POINT ( 'NONE',  ( 3.061616997868383141E-16, -27.75000000000000000, -5.000000000000000000 ) ) ;
#11695 = CARTESIAN_POINT ( 'NONE',  ( -3.753672977998669946, -3.033343224707661712, -5.749999998634407916 ) ) ;
#11696 = DIRECTION ( 'NONE',  ( 0.000000000000000000, 0.000000000000000000, -1.000000000000000000 ) ) ;
#11697 = DIRECTION ( 'NONE',  ( -0.8660254037844401509, 0.4999999999999973355, -0.000000000000000000 ) ) ;
#11698 = CARTESIAN_POINT ( 'NONE',  ( -5.000000000000000888, -23.68750000273119127, -2.071067811865475949 ) ) ;
#11699 = ORIENTED_EDGE ( 'NONE', *, *, #13618, .T. ) ;
#11700 = CARTESIAN_POINT ( 'NONE',  ( 3.152801135295366208, -25.56250000136559564, 3.152801135295367985 ) ) ;
#11701 = CARTESIAN_POINT ( 'NONE',  ( -0.2779000157839473517, -8.820699686765063774, -7.928862157988307402 ) ) ;
#11702 = ORIENTED_EDGE ( 'NONE', *, *, #5433, .F. ) ;
#11703 = VERTEX_POINT ( 'NONE', #7518 ) ;
#11704 = AXIS2_PLACEMENT_3D ( 'NONE', #3837, #127, #5373 ) ;
#11705 = DIRECTION ( 'NONE',  ( 0.000000000000000000, 0.4999999999999993339, -0.8660254037844390407 ) ) ;
#11706 = EDGE_CURVE ( 'NONE', #12259, #13050, #7681, .T. ) ;
#11707 = LINE ( 'NONE', #7438, #11242 ) ;
#11708 = EDGE_CURVE ( 'NONE', #3510, #12106, #10743, .T. ) ;
#11709 = VERTEX_POINT ( 'NONE', #15189 ) ;
#11710 = DIRECTION ( 'NONE',  ( 0.000000000000000000, 0.000000000000000000, -1.000000000000000000 ) ) ;
#11711 = CARTESIAN_POINT ( 'NONE',  ( -4.458734124999999437, -27.18750000136559564, -5.460374474430324690E-16 ) ) ;
#11712 = COLOUR_RGB ( '', 0.40784314, 0.44705882, 0.49803922) ;
#11713 = CARTESIAN_POINT ( 'NONE',  ( -1.415196051561583790, 4.795541693661363958, -6.624999997268815832 ) ) ;
#11714 = LINE ( 'NONE', #9319, #14170 ) ;
#11715 = PRODUCT_CONTEXT ( 'NONE', #11438, 'mechanical' ) ;
#11716 = AXIS2_PLACEMENT_3D ( 'NONE', #9461, #11791, #3090 ) ;
#11717 = TOROIDAL_SURFACE ( 'NONE', #14788, 4.000000000000000000, 0.2500000000000000000 ) ;
#11718 = CARTESIAN_POINT ( 'NONE',  ( 5.000000000000004441, -2.247904837838113790E-16, -7.920263044861759028 ) ) ;
#11719 = CARTESIAN_POINT ( 'NONE',  ( -3.033343224707664376, 3.753672977998667726, 0.7500000013655939712 ) ) ;
#11720 = EDGE_LOOP ( 'NONE', ( #1455, #8078 ) ) ;
#11722 = ORIENTED_EDGE ( 'NONE', *, *, #6255, .F. ) ;
#11721 = EDGE_CURVE ( 'NONE', #11920, #13100, #13830, .T. ) ;
#11723 = ADVANCED_FACE ( 'NONE', ( #11534 ), #2211, .T. ) ;
#11724 = PRODUCT_DEFINITION ( 'UNKNOWN', '', #6387, #13679 ) ;
#11725 = ORIENTED_EDGE ( 'NONE', *, *, #9988, .T. ) ;
#11726 = VECTOR ( 'NONE', #1418, 1000.000000000000000 ) ;
#11727 = CARTESIAN_POINT ( 'NONE',  ( 2.000000000000008882, 3.464101615137749945, 0.000000000000000000 ) ) ;
#11728 = CARTESIAN_POINT ( 'NONE',  ( -4.336808689942017736E-16, -8.660254037844399733, -9.999999999999998224 ) ) ;
#11729 = CIRCLE ( 'NONE', #13269, 9.999999999999994671 ) ;
#11730 = CARTESIAN_POINT ( 'NONE',  ( 4.209348295687701302, 3.401574460001765665, -6.812499997268814944 ) ) ;
#11731 = FILL_AREA_STYLE ('',( #12946 ) ) ;
#11732 = PLANE ( 'NONE',  #5119 ) ;
#11733 = DIRECTION ( 'NONE',  ( 1.000000000000000000, 0.000000000000000000, 0.000000000000000000 ) ) ;
#11734 = ORIENTED_EDGE ( 'NONE', *, *, #5295, .F. ) ;
#11735 = AXIS2_PLACEMENT_3D ( 'NONE', #9092, #13018, #761 ) ;
#11736 = DIRECTION ( 'NONE',  ( 1.000000000000000000, 0.000000000000000000, 0.000000000000000000 ) ) ;
#11737 = DIRECTION ( 'NONE',  ( 1.000000000000000000, 0.000000000000000000, 0.000000000000000000 ) ) ;
#11738 = CARTESIAN_POINT ( 'NONE',  ( 2.500000000000000000, -2.357898499370432610, 3.252606517456513302E-15 ) ) ;
#11739 = EDGE_CURVE ( 'NONE', #9005, #5616, #11005, .T. ) ;
#11740 = VERTEX_POINT ( 'NONE', #10264 ) ;
#11741 = FACE_OUTER_BOUND ( 'NONE', #13456, .T. ) ;
#11743 = ORIENTED_EDGE ( 'NONE', *, *, #10910, .F. ) ;
#11742 = PRODUCT_RELATED_PRODUCT_CATEGORY ( 'part', '', ( #13106 ) ) ;
#11744 = ADVANCED_FACE ( 'NONE', ( #8969 ), #7841, .F. ) ;
#11745 = EDGE_LOOP ( 'NONE', ( #9654, #6902, #2722, #15567 ) ) ;
#11746 = CARTESIAN_POINT ( 'NONE',  ( 3.535533905932738197, -23.00000000273118772, -3.535533905932738197 ) ) ;
#11747 = CARTESIAN_POINT ( 'NONE',  ( -3.436319922987618902, 2.634841920961291439, -3.531542292955721862 ) ) ;
#11748 = DIRECTION ( 'NONE',  ( 0.000000000000000000, 1.000000000000000000, -0.000000000000000000 ) ) ;
#11749 = CIRCLE ( 'NONE', #13816, 7.500000000000001776 ) ;
#11750 = AXIS2_PLACEMENT_3D ( 'NONE', #6059, #9684, #8499 ) ;
#11751 = DIRECTION ( 'NONE',  ( -0.000000000000000000, -0.000000000000000000, 1.000000000000000000 ) ) ;
#11752 = CARTESIAN_POINT ( 'NONE',  ( -5.725490332117410652, -3.000000000000000000, 9.916840153471811803 ) ) ;
#11753 = CARTESIAN_POINT ( 'NONE',  ( 2.499999999999999556, 0.000000000000000000, 3.469446951953614189E-15 ) ) ;
#11754 = CARTESIAN_POINT ( 'NONE',  ( 4.406842699996126989, -6.115962218725296218, -6.661067097207817866E-15 ) ) ;
#11755 = LINE ( 'NONE', #3045, #14021 ) ;
#11756 = CARTESIAN_POINT ( 'NONE',  ( -4.403473400622100797, -6.117907484625868086, -4.528238136021488035E-15 ) ) ;
#11757 = CARTESIAN_POINT ( 'NONE',  ( -3.152801135295367096, -28.31250000136559564, -3.152801135295367541 ) ) ;
#11758 = CARTESIAN_POINT ( 'NONE',  ( 0.5093500532425063732, 4.799145180956616130, -0.1249999986344088321 ) ) ;
#11759 = ORIENTED_EDGE ( 'NONE', *, *, #8484, .T. ) ;
#11760 = VECTOR ( 'NONE', #14514, 1000.000000000000000 ) ;
#11761 = UNCERTAINTY_MEASURE_WITH_UNIT (LENGTH_MEASURE( 1.000000000000000082E-05 ), #13754, 'distance_accuracy_value', 'NONE');
#11762 = DIRECTION ( 'NONE',  ( 0.000000000000000000, 0.000000000000000000, -1.000000000000000000 ) ) ;
#11763 = EDGE_LOOP ( 'NONE', ( #9810, #15059 ) ) ;
#11764 = ORIENTED_EDGE ( 'NONE', *, *, #4257, .F. ) ;
#11765 = CIRCLE ( 'NONE', #12279, 10.00000000000000000 ) ;
#11766 = EDGE_CURVE ( 'NONE', #8391, #9721, #12420, .T. ) ;
#11767 = CARTESIAN_POINT ( 'NONE',  ( 1.846868145590736310, -27.87500000136559564, 4.458734124999999437 ) ) ;
#11768 = DIRECTION ( 'NONE',  ( 0.8660254037844407060, -0.4999999999999966693, 0.000000000000000000 ) ) ;
#11769 = CARTESIAN_POINT ( 'NONE',  ( 9.999999999999891642, -13.00000000000000178, -14.82050807568883677 ) ) ;
#11770 = AXIS2_PLACEMENT_3D ( 'NONE', #13030, #11737, #844 ) ;
#11771 = DIRECTION ( 'NONE',  ( 1.000000000000000000, 0.000000000000000000, 0.000000000000000000 ) ) ;
#11772 = CARTESIAN_POINT ( 'NONE',  ( -0.5093500532425060401, -4.799145180956616130, -6.624999998634407916 ) ) ;
#11773 = CARTESIAN_POINT ( 'NONE',  ( 2.875844205642646756, -3.000000000000000000, 48.98110827882563711 ) ) ;
#11774 = CIRCLE ( 'NONE', #9215, 25.00000000000000000 ) ;
#11775 = CARTESIAN_POINT ( 'NONE',  ( 3.535533905932736864, -24.12500000000000000, 3.535533905932738641 ) ) ;
#11776 = CIRCLE ( 'NONE', #11007, 2.649999999999992806 ) ;
#11777 = CARTESIAN_POINT ( 'NONE',  ( 4.799145180956616130, -0.5093500532425063732, -6.374999998634407028 ) ) ;
#11778 = CARTESIAN_POINT ( 'NONE',  ( 0.000000000000000000, -13.00000000000000178, 0.000000000000000000 ) ) ;
#11779 = LINE ( 'NONE', #732, #3037 ) ;
#11780 = CARTESIAN_POINT ( 'NONE',  ( -5.000000000000000000, -21.62500000273118772, -6.123233995736766282E-16 ) ) ;
#11781 = ORIENTED_EDGE ( 'NONE', *, *, #12839, .F. ) ;
#11782 = CARTESIAN_POINT ( 'NONE',  ( 3.152801135295366208, -26.56250000136559564, 3.152801135295367985 ) ) ;
#11783 = LINE ( 'NONE', #6637, #12515 ) ;
#11784 = ORIENTED_EDGE ( 'NONE', *, *, #4510, .T. ) ;
#11785 = AXIS2_PLACEMENT_3D ( 'NONE', #3667, #3427, #7165 ) ;
#11786 = ORIENTED_EDGE ( 'NONE', *, *, #4164, .F. ) ;
#11787 = CARTESIAN_POINT ( 'NONE',  ( 7.500000000000000000, -2.571118828324946648, -0.3627527587569098766 ) ) ;
#11788 = CARTESIAN_POINT ( 'NONE',  ( 2.071067811865492825, -28.93750000273118772, -4.999999999999983125 ) ) ;
#11789 = PRODUCT_DEFINITION_FORMATION_WITH_SPECIFIED_SOURCE ( 'ANY', '', #609, .NOT_KNOWN. ) ;
#11790 = ORIENTED_EDGE ( 'NONE', *, *, #7093, .T. ) ;
#11791 = DIRECTION ( 'NONE',  ( -0.000000000000000000, 0.000000000000000000, -1.000000000000000000 ) ) ;
#11792 = AXIS2_PLACEMENT_3D ( 'NONE', #212, #11420, #15151 ) ;
#11793 = DIRECTION ( 'NONE',  ( 0.000000000000000000, 0.000000000000000000, -1.000000000000000000 ) ) ;
#11794 = CARTESIAN_POINT ( 'NONE',  ( 1.846868145590735200, -26.50000000136559208, -4.458734125000000326 ) ) ;
#11795 = CARTESIAN_POINT ( 'NONE',  ( 25.00000000000000000, 0.000000000000000000, 0.000000000000000000 ) ) ;
#11796 = EDGE_CURVE ( 'NONE', #10466, #9335, #14611, .T. ) ;
#11797 = CARTESIAN_POINT ( 'NONE',  ( 1.415196051561583790, -4.795541693661363958, -4.250000000000000000 ) ) ;
#11798 = CONTEXT_DEPENDENT_SHAPE_REPRESENTATION ( #3312, #2148 ) ;
#11799 = AXIS2_PLACEMENT_3D ( 'NONE', #12119, #10764, #10684 ) ;
#11800 = CARTESIAN_POINT ( 'NONE',  ( 4.276409079477644148, 1.261996585732577891, -7.562499998634407916 ) ) ;
#11801 = CARTESIAN_POINT ( 'NONE',  ( 3.916244202832140253, -2.131511515620588160, 0.3125000013655919728 ) ) ;
#11802 = ORIENTED_EDGE ( 'NONE', *, *, #925, .F. ) ;
#11803 = VERTEX_POINT ( 'NONE', #4105 ) ;
#11804 = CARTESIAN_POINT ( 'NONE',  ( -4.000000000000000000, 2.309401076758498483, -0.4999999999999927280 ) ) ;
#11805 = ORIENTED_EDGE ( 'NONE', *, *, #2500, .T. ) ;
#11806 = ITEM_DEFINED_TRANSFORMATION ( 'NONE', 'NONE', #15873,  #3223 ) ;
#11807 = CIRCLE ( 'NONE', #5380, 39.99999999999999289 ) ;
#11808 = LINE ( 'NONE', #9327, #9425 ) ;
#11809 =( BOUNDED_CURVE ( )  B_SPLINE_CURVE ( 2, ( #8068, #12963, #5706, #552, #13044, #1984, #15337, #4416, #4250 ),
 .UNSPECIFIED., .F., .F. ) 
 B_SPLINE_CURVE_WITH_KNOTS ( ( 3, 2, 2, 2, 3 ),
 ( 0.8750000000000000000, 0.8874999999999999556, 0.9000000000000001332, 0.9125000000000000888, 0.9250000000000002665 ),
 .UNSPECIFIED. ) 
 CURVE ( )  GEOMETRIC_REPRESENTATION_ITEM ( )  RATIONAL_B_SPLINE_CURVE ( ( 1.000000000000000000, 0.9238795325112867385, 1.000000000000000000, 0.9238795325112867385, 1.000000000000000000, 0.9238795325112867385, 1.000000000000000000, 0.9238795325112854062, 1.000000000000001332 ) ) 
 REPRESENTATION_ITEM ( '' )  );
#11810 = DIRECTION ( 'NONE',  ( -0.000000000000000000, -1.000000000000000000, -0.000000000000000000 ) ) ;
#11811 = VECTOR ( 'NONE', #1344, 1000.000000000000000 ) ;
#11812 = EDGE_CURVE ( 'NONE', #13331, #7289, #14863, .T. ) ;
#11813 = DIRECTION ( 'NONE',  ( -0.000000000000000000, -0.000000000000000000, 1.000000000000000000 ) ) ;
#11814 = ADVANCED_FACE ( 'NONE', ( #11378 ), #6383, .T. ) ;
#11815 = AXIS2_PLACEMENT_3D ( 'NONE', #8342, #9544, #9776 ) ;
#11816 = CARTESIAN_POINT ( 'NONE',  ( 2.390265326283148806, 4.391654775818395251, -8.749999997268814056 ) ) ;
#11817 = LINE ( 'NONE', #3184, #9516 ) ;
#11818 = DIRECTION ( 'NONE',  ( 0.000000000000000000, 0.000000000000000000, 1.000000000000000000 ) ) ;
#11819 = ORIENTED_EDGE ( 'NONE', *, *, #6445, .F. ) ;
#11820 = DIRECTION ( 'NONE',  ( -1.000000000000000000, -0.000000000000000000, -0.000000000000000000 ) ) ;
#11821 = DIRECTION ( 'NONE',  ( 0.000000000000000000, 0.000000000000000000, 1.000000000000000000 ) ) ;
#11822 = CIRCLE ( 'NONE', #4871, 40.00000000000001421 ) ;
#11823 = CARTESIAN_POINT ( 'NONE',  ( 0.000000000000000000, 0.000000000000000000, -25.03750572909317285 ) ) ;
#11824 = ORIENTED_EDGE ( 'NONE', *, *, #601, .F. ) ;
#11825 = CARTESIAN_POINT ( 'NONE',  ( 5.000000000000000000, -27.06250000000000000, 2.071067811865478614 ) ) ;
#11826 = VERTEX_POINT ( 'NONE', #11301 ) ;
#11827 = VERTEX_POINT ( 'NONE', #15349 ) ;
#11828 = CARTESIAN_POINT ( 'NONE',  ( 4.276409079477644148, 1.261996585732577891, -0.5624999986344088043 ) ) ;
#11829 = CARTESIAN_POINT ( 'NONE',  ( 0.02448733951239481094, 4.877042772274728044, -3.751161874094022242 ) ) ;
#11830 = VECTOR ( 'NONE', #2953, 1000.000000000000114 ) ;
#11831 = AXIS2_PLACEMENT_3D ( 'NONE', #10904, #15847, #4764 ) ;
#11832 = CARTESIAN_POINT ( 'NONE',  ( 4.795541693661363958, 1.415196051561583790, -3.469446951953614189E-15 ) ) ;
#11833 = EDGE_CURVE ( 'NONE', #7493, #3061, #789, .T. ) ;
#11834 = CARTESIAN_POINT ( 'NONE',  ( 35.00000000000000000, 40.00000000000000000, -5.999999999999991118 ) ) ;
#11835 = FACE_BOUND ( 'NONE', #11559, .T. ) ;
#11836 = EDGE_CURVE ( 'NONE', #10306, #5664, #14612, .T. ) ;
#11837 = DIRECTION ( 'NONE',  ( 0.000000000000000000, -1.000000000000000000, 0.000000000000000000 ) ) ;
#11838 = DIRECTION ( 'NONE',  ( 1.000000000000000000, 0.000000000000000000, 0.000000000000000000 ) ) ;
#11839 = CARTESIAN_POINT ( 'NONE',  ( 6.000000000000000000, -13.00000000000000178, 1.500000000000000000 ) ) ;
#11840 = CARTESIAN_POINT ( 'NONE',  ( 42.02221399786069611, -1.230770033143087371E-15, 1.075528555105620399E-13 ) ) ;
#11841 = CARTESIAN_POINT ( 'NONE',  ( 3.152801135295367541, -29.56250000136559208, -3.152801135295367541 ) ) ;
#11842 = CARTESIAN_POINT ( 'NONE',  ( -0.5093500532425060401, -4.799145180956616130, -1.624999998634406362 ) ) ;
#11843 = ORIENTED_EDGE ( 'NONE', *, *, #1593, .F. ) ;
#11844 = VECTOR ( 'NONE', #9476, 1000.000000000000114 ) ;
#11845 = CYLINDRICAL_SURFACE ( 'NONE', #3248, 2.649999999999992806 ) ;
#11846 = VERTEX_POINT ( 'NONE', #9130 ) ;
#11847 = ORIENTED_EDGE ( 'NONE', *, *, #5435, .T. ) ;
#11848 =( NAMED_UNIT ( * ) PLANE_ANGLE_UNIT ( ) SI_UNIT ( $, .RADIAN. ) );
#11849 = CARTESIAN_POINT ( 'NONE',  ( 4.458734124999999437, -27.75000000136559564, 1.846868145590737864 ) ) ;
#11850 = DIRECTION ( 'NONE',  ( -0.000000000000000000, 1.000000000000000000, -0.000000000000000000 ) ) ;
#11851 = DIRECTION ( 'NONE',  ( 0.8660254037844402619, -0.4999999999999973910, 0.000000000000000000 ) ) ;
#11852 = PLANE ( 'NONE',  #5400 ) ;
#11853 = EDGE_CURVE ( 'NONE', #5239, #1848, #8005, .T. ) ;
#11854 = CARTESIAN_POINT ( 'NONE',  ( -4.276409079477644148, -1.261996585732578335, -6.812499998634407028 ) ) ;
#11855 = CARTESIAN_POINT ( 'NONE',  ( 3.876648187198773687, -3.253774389711713511, 48.74739051362634257 ) ) ;
#11856 = EDGE_CURVE ( 'NONE', #14753, #13545, #4398, .T. ) ;
#11857 = CARTESIAN_POINT ( 'NONE',  ( -9.184850993605147944E-16, -27.25000000000000000, 5.000000000000000000 ) ) ;
#11858 = CARTESIAN_POINT ( 'NONE',  ( 3.401574460001763001, -4.209348295687703967, 0.8124999999999960032 ) ) ;
#11859 = CARTESIAN_POINT ( 'NONE',  ( -6.765421556309547668E-13, 37.00000000000000000, 67.49999999999930367 ) ) ;
#11860 = DIRECTION ( 'NONE',  ( 0.000000000000000000, 1.000000000000000000, 0.000000000000000000 ) ) ;
#11861 = CARTESIAN_POINT ( 'NONE',  ( -8.190561711645485556E-16, -29.68750000136559208, 4.458734124999999437 ) ) ;
#11862 = ORIENTED_EDGE ( 'NONE', *, *, #8608, .T. ) ;
#11863 = DIRECTION ( 'NONE',  ( -0.000000000000000000, 1.000000000000000000, -0.000000000000000000 ) ) ;
#11864 =( REPRESENTATION_RELATIONSHIP ('NONE','NONE', #4176, #4696 ) REPRESENTATION_RELATIONSHIP_WITH_TRANSFORMATION ( #15550 )SHAPE_REPRESENTATION_RELATIONSHIP( ) );
#11865 = DIRECTION ( 'NONE',  ( -1.000000000000000000, -0.000000000000000000, -0.000000000000000000 ) ) ;
#11866 = ORIENTED_EDGE ( 'NONE', *, *, #12068, .F. ) ;
#11867 = ORIENTED_EDGE ( 'NONE', *, *, #7211, .T. ) ;
#11868 = CARTESIAN_POINT ( 'NONE',  ( 5.000000000000095923, 0.7223674278660565662, -3.896799362785971610 ) ) ;
#11869 = CARTESIAN_POINT ( 'NONE',  ( -4.458734125000000326, -27.00000000136559208, -1.846868145590735644 ) ) ;
#11870 = CARTESIAN_POINT ( 'NONE',  ( 1.415196051561583790, -4.795541693661363958, -7.124999997268815832 ) ) ;
#11871 = VERTEX_POINT ( 'NONE', #10501 ) ;
#11872 = DIRECTION ( 'NONE',  ( 0.000000000000000000, 0.000000000000000000, 1.000000000000000000 ) ) ;
#11873 = CARTESIAN_POINT ( 'NONE',  ( -49.14213562373093680, -30.85786437626904899, 17.49999999999999645 ) ) ;
#11874 = EDGE_CURVE ( 'NONE', #14954, #13586, #1914, .T. ) ;
#11875 = CARTESIAN_POINT ( 'NONE',  ( -3.152801135295367096, -27.31250000136559564, -3.152801135295367541 ) ) ;
#11876 = CARTESIAN_POINT ( 'NONE',  ( 1.274258131564866448, 3.883108878240963513, -3.220599429844046568 ) ) ;
#11877 = CARTESIAN_POINT ( 'NONE',  ( 1.415196051561583790, -4.795541693661363958, -0.1249999972688167760 ) ) ;
#11878 = CYLINDRICAL_SURFACE ( 'NONE', #13799, 9.999999999999994671 ) ;
#11879 = COLOUR_RGB ( '', 0.66274510, 0.83137255, 0.94901961) ;
#11880 = DIRECTION ( 'NONE',  ( 1.000000000000000000, 0.000000000000000000, 0.000000000000000000 ) ) ;
#11881 = ORIENTED_EDGE ( 'NONE', *, *, #15691, .T. ) ;
#11882 = ORIENTED_EDGE ( 'NONE', *, *, #5864, .T. ) ;
#11883 = CARTESIAN_POINT ( 'NONE',  ( -4.000000000000000000, 1.941961291383472732, -0.3515519931180205448 ) ) ;
#11884 = VERTEX_POINT ( 'NONE', #797 ) ;
#11885 = EDGE_CURVE ( 'NONE', #3698, #7837, #9440, .T. ) ;
#11886 = DIRECTION ( 'NONE',  ( -1.000000000000000000, 0.000000000000000000, 0.000000000000000000 ) ) ;
#11887 = DIRECTION ( 'NONE',  ( -0.000000000000000000, -0.000000000000000000, -1.000000000000000000 ) ) ;
#11888 = CARTESIAN_POINT ( 'NONE',  ( 1.261996585732578113, -4.276409079477644148, 0.4375000013655920839 ) ) ;
#11889 = DIRECTION ( 'NONE',  ( 6.123233995736766036E-17, 1.000000000000000000, 0.000000000000000000 ) ) ;
#11890 = CARTESIAN_POINT ( 'NONE',  ( 1.415196051561583790, -4.795541693661363958, -6.124999997268814944 ) ) ;
#11891 = CARTESIAN_POINT ( 'NONE',  ( -19.99999999999956657, -20.00000000000000000, 8.786575603324269439E-13 ) ) ;
#11892 = CARTESIAN_POINT ( 'NONE',  ( -1.908195823574487804E-14, -8.660254037844392627, -1.000000000000000888 ) ) ;
#11893 = DIRECTION ( 'NONE',  ( 0.9396926207859138680, 1.150791560227856926E-16, -0.3420201433256536139 ) ) ;
#11894 = VERTEX_POINT ( 'NONE', #14041 ) ;
#11895 = LINE ( 'NONE', #15560, #11303 ) ;
#11896 = CARTESIAN_POINT ( 'NONE',  ( 2.390265326283148806, 4.391654775818395251, -2.749999997268815832 ) ) ;
#11897 = CARTESIAN_POINT ( 'NONE',  ( 0.000000000000000000, 0.000000000000000000, 0.000000000000000000 ) ) ;
#11898 = ORIENTED_EDGE ( 'NONE', *, *, #9462, .F. ) ;
#11899 = DIRECTION ( 'NONE',  ( 0.000000000000000000, -1.000000000000000000, 0.000000000000000000 ) ) ;
#11900 = ORIENTED_EDGE ( 'NONE', *, *, #11025, .F. ) ;
#11901 = ORIENTED_EDGE ( 'NONE', *, *, #11739, .F. ) ;
#11902 = CARTESIAN_POINT ( 'NONE',  ( 2.071067811865476394, -23.31250000273118772, 5.000000000000000000 ) ) ;
#11903 = ADVANCED_FACE ( 'NONE', ( #7917 ), #12818, .F. ) ;
#11904 = CARTESIAN_POINT ( 'NONE',  ( -99.99999999999998579, -25.00000000000000711, -17.50000000000000000 ) ) ;
#11905 = VECTOR ( 'NONE', #14505, 1000.000000000000000 ) ;
#11906 = EDGE_CURVE ( 'NONE', #5083, #12918, #6364, .T. ) ;
#11907 =( BOUNDED_CURVE ( )  B_SPLINE_CURVE ( 2, ( #12187, #14316, #2342, #12117, #2031, #13092, #7285, #6977, #8347 ),
 .UNSPECIFIED., .F., .F. ) 
 B_SPLINE_CURVE_WITH_KNOTS ( ( 3, 2, 2, 2, 3 ),
 ( 0.07500000000000006661, 0.08750000000000007772, 0.1000000000000000888, 0.1125000000000000999, 0.1250000000000001110 ),
 .UNSPECIFIED. ) 
 CURVE ( )  GEOMETRIC_REPRESENTATION_ITEM ( )  RATIONAL_B_SPLINE_CURVE ( ( 0.9999999999999995559, 0.9238795325112871826, 1.000000000000000000, 0.9238795325112867385, 1.000000000000000000, 0.9238795325112867385, 1.000000000000000000, 0.9238795325112860723, 1.000000000000000666 ) ) 
 REPRESENTATION_ITEM ( '' )  );
#11908 = CARTESIAN_POINT ( 'NONE',  ( -6.901579824520448270, 4.675625068323816969, -0.7022220667781353676 ) ) ;
#11909 = DIRECTION ( 'NONE',  ( 0.000000000000000000, 1.000000000000000000, 0.000000000000000000 ) ) ;
#11910 = FACE_BOUND ( 'NONE', #15705, .T. ) ;
#11911 = CARTESIAN_POINT ( 'NONE',  ( 2.500000000000000000, -1.178949249685213863, 2.042000000000002924 ) ) ;
#11912 = CARTESIAN_POINT ( 'NONE',  ( 5.047120108843203390, -5.746297884371400322, -0.1007566405101857077 ) ) ;
#11913 = CARTESIAN_POINT ( 'NONE',  ( 23.49999999999956657, -8.782289339527253835E-13, 0.000000000000000000 ) ) ;
#11914 = DIRECTION ( 'NONE',  ( -0.9999824063907751803, -0.005931855436079011210, 0.000000000000000000 ) ) ;
#11915 = CARTESIAN_POINT ( 'NONE',  ( -1.846868145590734756, -28.37500000136559564, -4.458734124999999437 ) ) ;
#11916 = CARTESIAN_POINT ( 'NONE',  ( 4.799145180956616130, -0.5093500532425063732, 1.625000001365592528 ) ) ;
#11917 = ORIENTED_EDGE ( 'NONE', *, *, #14232, .T. ) ;
#11918 = CARTESIAN_POINT ( 'NONE',  ( 6.658902113223716057, 5.287118297637872999, -7.776713651266099703 ) ) ;
#11919 = ORIENTED_EDGE ( 'NONE', *, *, #1995, .F. ) ;
#11920 = VERTEX_POINT ( 'NONE', #1763 ) ;
#11921 =( LENGTH_UNIT ( ) NAMED_UNIT ( * ) SI_UNIT ( .MILLI., .METRE. ) );
#11922 = ORIENTED_EDGE ( 'NONE', *, *, #11833, .F. ) ;
#11923 = CARTESIAN_POINT ( 'NONE',  ( 3.152801135295366208, -27.81250000136559564, 3.152801135295367985 ) ) ;
#11924 = CARTESIAN_POINT ( 'NONE',  ( -4.391654775818395251, 2.390265326283148806, -7.625000000000003553 ) ) ;
#11925 = EDGE_CURVE ( 'NONE', #10564, #4014, #15587, .T. ) ;
#11926 = CARTESIAN_POINT ( 'NONE',  ( 5.000000000000000888, 0.000000000000000000, 0.000000000000000000 ) ) ;
#11927 = CARTESIAN_POINT ( 'NONE',  ( 4.276409079477644148, 1.261996585732577891, -5.312499998634406140 ) ) ;
#11928 = DIRECTION ( 'NONE',  ( 1.000000000000000000, 0.000000000000000000, 0.000000000000000000 ) ) ;
#11929 = CARTESIAN_POINT ( 'NONE',  ( -28.86751345948126612, -20.00000000000000000, -18.00000000000000711 ) ) ;
#11930 = CARTESIAN_POINT ( 'NONE',  ( 0.5711823568785989735, 5.381735091635026613, 1.187499999999998224 ) ) ;
#11931 = DIRECTION ( 'NONE',  ( -0.8660254037844402619, 0.4999999999999973355, 0.000000000000000000 ) ) ;
#11932 = CARTESIAN_POINT ( 'NONE',  ( 33.48631561300354065, -3.000000000000000000, 14.00000000000909850 ) ) ;
#11933 = CARTESIAN_POINT ( 'NONE',  ( -4.458734125000000326, -30.00000000136559564, -1.846868145590735644 ) ) ;
#11934 = ORIENTED_EDGE ( 'NONE', *, *, #15814, .T. ) ;
#11935 = CARTESIAN_POINT ( 'NONE',  ( 1.846868145590735200, -23.25000000136559564, -4.458734124999999437 ) ) ;
#11936 = AXIS2_PLACEMENT_3D ( 'NONE', #3859, #8959, #13947 ) ;
#11937 = CARTESIAN_POINT ( 'NONE',  ( 0.000000000000000000, 0.000000000000000000, 0.000000000000000000 ) ) ;
#11938 = ORIENTED_EDGE ( 'NONE', *, *, #7796, .T. ) ;
#11939 = ORIENTED_EDGE ( 'NONE', *, *, #11706, .T. ) ;
#11940 = CARTESIAN_POINT ( 'NONE',  ( 6.000000000000000000, -13.00000000000000178, 1.500000000000000000 ) ) ;
#11941 = CARTESIAN_POINT ( 'NONE',  ( -4.458734125000001214, -29.87500000136559564, 1.846868145590734089 ) ) ;
#11942 = EDGE_CURVE ( 'NONE', #11577, #2543, #563, .T. ) ;
#11943 = CARTESIAN_POINT ( 'NONE',  ( 5.000000000000004441, -2.247904837838113790E-16, -6.920263044861760804 ) ) ;
#11944 = EDGE_CURVE ( 'NONE', #7180, #5811, #2735, .T. ) ;
#11945 = EDGE_CURVE ( 'NONE', #12106, #8217, #12902, .T. ) ;
#11946 = ORIENTED_EDGE ( 'NONE', *, *, #12395, .T. ) ;
#11947 = CARTESIAN_POINT ( 'NONE',  ( 4.795541693661363958, 1.415196051561583790, -3.469446951953614189E-15 ) ) ;
#11948 = PRODUCT_DEFINITION_SHAPE ( 'NONE', 'NONE',  #13413 ) ;
#11949 = DIRECTION ( 'NONE',  ( -0.000000000000000000, 1.000000000000000000, -0.000000000000000000 ) ) ;
#11950 = CARTESIAN_POINT ( 'NONE',  ( 0.000000000000000000, 40.00000000000000000, 0.000000000000000000 ) ) ;
#11951 = CARTESIAN_POINT ( 'NONE',  ( -4.458734124999999437, -28.18750000136559564, -5.460374474430324690E-16 ) ) ;
#11952 = LINE ( 'NONE', #13241, #10382 ) ;
#11953 = LINE ( 'NONE', #8279, #6428 ) ;
#11954 = CARTESIAN_POINT ( 'NONE',  ( -3.535533905932738641, -30.50000000273118772, 3.535533905932737309 ) ) ;
#11955 = CARTESIAN_POINT ( 'NONE',  ( -21.01110699893060030, 0.000000000000000000, 39.04230484541323420 ) ) ;
#11956 = EDGE_LOOP ( 'NONE', ( #12693, #5556, #6880, #12814 ) ) ;
#11957 = SURFACE_STYLE_USAGE ( .BOTH. , #4622 ) ;
#11958 = ORIENTED_EDGE ( 'NONE', *, *, #86, .F. ) ;
#11959 = LINE ( 'NONE', #10451, #4886 ) ;
#11960 = EDGE_CURVE ( 'NONE', #7410, #757, #5646, .T. ) ;
#11961 = ORIENTED_EDGE ( 'NONE', *, *, #2813, .F. ) ;
#11962 = DIRECTION ( 'NONE',  ( -0.000000000000000000, -0.000000000000000000, -1.000000000000000000 ) ) ;
#11963 = AXIS2_PLACEMENT_3D ( 'NONE', #8259, #9448, #10512 ) ;
#11964 = CARTESIAN_POINT ( 'NONE',  ( -10.12668159690567649, 1.240160820363494356E-15, -9.226681596905677907 ) ) ;
#11965 = CARTESIAN_POINT ( 'NONE',  ( -4.799145180956616130, 0.5093500532425063732, 0.1250000013655913900 ) ) ;
#11966 = DIRECTION ( 'NONE',  ( 6.123233995736766036E-17, 1.000000000000000000, 0.000000000000000000 ) ) ;
#11967 = CARTESIAN_POINT ( 'NONE',  ( -2.131511515620587272, -3.916244202832140253, 0.06250000136559172303 ) ) ;
#11968 = CYLINDRICAL_SURFACE ( 'NONE', #13344, 5.000000000000000888 ) ;
#11969 = DIRECTION ( 'NONE',  ( -0.5000000000000000000, 8.673617379884033500E-16, 0.8660254037844385966 ) ) ;
#11970 = ORIENTED_EDGE ( 'NONE', *, *, #4198, .T. ) ;
#11971 = FACE_OUTER_BOUND ( 'NONE', #7718, .T. ) ;
#11972 = DIRECTION ( 'NONE',  ( 0.000000000000000000, 0.000000000000000000, 1.000000000000000000 ) ) ;
#11973 = ORIENTED_EDGE ( 'NONE', *, *, #11706, .F. ) ;
#11974 = CARTESIAN_POINT ( 'NONE',  ( 5.000000000000004441, 0.000000000000000000, 4.250000000000000000 ) ) ;
#11975 = EDGE_LOOP ( 'NONE', ( #8588, #3846, #55, #8783, #13742, #15527, #2109, #1133 ) ) ;
#11976 = VECTOR ( 'NONE', #10082, 1000.000000000000000 ) ;
#11977 = ORIENTED_EDGE ( 'NONE', *, *, #6445, .T. ) ;
#11978 = CARTESIAN_POINT ( 'NONE',  ( -3.535533905932738641, -30.37500000000000000, 3.535533905932737309 ) ) ;
#11979 = CARTESIAN_POINT ( 'NONE',  ( -60.00000000000000000, -5.000000000000000000, -20.00000000000000711 ) ) ;
#11980 = MECHANICAL_DESIGN_GEOMETRIC_PRESENTATION_REPRESENTATION (  '', ( #14323 ), #5029 ) ;
#11981 =( GEOMETRIC_REPRESENTATION_CONTEXT ( 3 ) GLOBAL_UNCERTAINTY_ASSIGNED_CONTEXT ( ( #15507 ) ) GLOBAL_UNIT_ASSIGNED_CONTEXT ( ( #15700, #3471, #2264 ) ) REPRESENTATION_CONTEXT ( 'NONE', 'WORKASPACE' ) );
#11982 = CARTESIAN_POINT ( 'NONE',  ( -7.922281120364393914, 4.573931137438272287, -8.047472243342932430 ) ) ;
#11983 = CARTESIAN_POINT ( 'NONE',  ( 1.415196051561583790, -4.795541693661363958, -2.250000000000001776 ) ) ;
#11984 = VECTOR ( 'NONE', #834, 1000.000000000000000 ) ;
#11985 = CARTESIAN_POINT ( 'NONE',  ( 33.48631561299831105, -3.000000000000000000, -13.99999999999999645 ) ) ;
#11986 = CARTESIAN_POINT ( 'NONE',  ( 2.390265326283148806, 4.391654775818395251, -0.7499999972688138339 ) ) ;
#11987 = DIRECTION ( 'NONE',  ( 0.000000000000000000, -1.000000000000000000, 0.000000000000000000 ) ) ;
#11988 = EDGE_CURVE ( 'NONE', #10616, #1037, #11498, .T. ) ;
#11989 = CARTESIAN_POINT ( 'NONE',  ( 0.000000000000000000, 0.000000000000000000, -8.499999999999996447 ) ) ;
#11990 = CARTESIAN_POINT ( 'NONE',  ( 1.846868145590735200, -30.50000000136559919, -4.458734124999999437 ) ) ;
#11991 = CARTESIAN_POINT ( 'NONE',  ( 3.916244202832140253, -2.131511515620588160, 0.5625000013655921949 ) ) ;
#11992 = VERTEX_POINT ( 'NONE', #5793 ) ;
#11993 = CARTESIAN_POINT ( 'NONE',  ( 2.467663300281917732E-15, 37.00000000000000000, -64.85000000000000853 ) ) ;
#11994 = ORIENTED_EDGE ( 'NONE', *, *, #7326, .T. ) ;
#11995 = VERTEX_POINT ( 'NONE', #3520 ) ;
#11996 =( BOUNDED_CURVE ( )  B_SPLINE_CURVE ( 2, ( #5512, #1791, #667, #7950, #429, #5354, #2915, #7866, #15377, #4299, #13168 ),
 .UNSPECIFIED., .F., .F. ) 
 B_SPLINE_CURVE_WITH_KNOTS ( ( 3, 2, 2, 2, 2, 3 ),
 ( 0.1545872658012772960, 0.1625000000000000056, 0.1749999999999999889, 0.1875000000000000000, 0.2000000000000000111, 0.2045872658012772849 ),
 .UNSPECIFIED. ) 
 CURVE ( )  GEOMETRIC_REPRESENTATION_ITEM ( )  RATIONAL_B_SPLINE_CURVE ( ( 0.9646335149384808183, 0.9518143178943438976, 1.000000000000000000, 0.9238795325112867385, 1.000000000000000000, 0.9238795325112867385, 1.000000000000000000, 0.9238795325112867385, 1.000000000000000000, 0.9720652146169430630, 0.9646335149384808183 ) ) 
 REPRESENTATION_ITEM ( '' )  );
#11998 = VECTOR ( 'NONE', #5076, 1000.000000000000000 ) ;
#11997 = SURFACE_SIDE_STYLE ('',( #12156 ) ) ;
#11999 = ORIENTED_EDGE ( 'NONE', *, *, #10686, .F. ) ;
#12000 = CARTESIAN_POINT ( 'NONE',  ( 4.458734124999999437, -26.68750000136559564, 0.000000000000000000 ) ) ;
#12001 = CYLINDRICAL_SURFACE ( 'NONE', #12015, 5.000000000000000000 ) ;
#12002 = VECTOR ( 'NONE', #9770, 1000.000000000000000 ) ;
#12003 = AXIS2_PLACEMENT_3D ( 'NONE', #10903, #1118, #5980 ) ;
#12004 = CARTESIAN_POINT ( 'NONE',  ( 21.99999999999956657, -8.786575603324269439E-13, 0.000000000000000000 ) ) ;
#12005 = CARTESIAN_POINT ( 'NONE',  ( -90.00000000000000000, -35.00000000000000711, 17.50000000000000000 ) ) ;
#12006 = CARTESIAN_POINT ( 'NONE',  ( 2.290893957444128645E-15, 4.647089433458768681, -3.572167766733382877 ) ) ;
#12007 = CARTESIAN_POINT ( 'NONE',  ( -2.071067811865475061, -23.68750000000000355, -5.000000000000000888 ) ) ;
#12008 = CONICAL_SURFACE ( 'NONE', #7137, 5.560781378645573980, 1.221730476396046816 ) ;
#12009 = CARTESIAN_POINT ( 'NONE',  ( 3.753672977998667726, 3.033343224707664376, -8.249999998634409692 ) ) ;
#12010 = PLANE ( 'NONE',  #6566 ) ;
#12011 = ADVANCED_FACE ( 'NONE', ( #5878 ), #10812, .F. ) ;
#12012 = CARTESIAN_POINT ( 'NONE',  ( 1.023706143822011194, -4.792166261265705884, -0.07488405613504552083 ) ) ;
#12013 = EDGE_CURVE ( 'NONE', #6779, #6965, #3607, .T. ) ;
#12014 = CARTESIAN_POINT ( 'NONE',  ( -3.152801135295367096, -31.06250000136559564, -3.152801135295367541 ) ) ;
#12015 = AXIS2_PLACEMENT_3D ( 'NONE', #3374, #8321, #951 ) ;
#12016 = VERTEX_POINT ( 'NONE', #13523 ) ;
#12017 = EDGE_LOOP ( 'NONE', ( #7292, #14246, #11862, #14342 ) ) ;
#12018 = ORIENTED_EDGE ( 'NONE', *, *, #1639, .F. ) ;
#12019 = DIRECTION ( 'NONE',  ( -0.000000000000000000, 0.000000000000000000, 1.000000000000000000 ) ) ;
#12020 = CARTESIAN_POINT ( 'NONE',  ( 4.458734124999999437, -29.43750000136559208, 0.000000000000000000 ) ) ;
#12021 = DIRECTION ( 'NONE',  ( 0.000000000000000000, 0.000000000000000000, 1.000000000000000000 ) ) ;
#12022 = VECTOR ( 'NONE', #221, 1000.000000000000000 ) ;
#12023 = VERTEX_POINT ( 'NONE', #6038 ) ;
#12024 = CARTESIAN_POINT ( 'NONE',  ( -2.071067811865503483, -24.81250000273118772, -4.999999999999971578 ) ) ;
#12025 = CIRCLE ( 'NONE', #2469, 2.700000000000000622 ) ;
#12026 = CLOSED_SHELL ( 'NONE', ( #15533, #4443, #1557, #9354, #10486, #13035, #15442, #12658, #1658, #6562, #276, #11903, #13619, #3795, #4661, #13095 ) ) ;
#12027 = CARTESIAN_POINT ( 'NONE',  ( -116.3391301858327296, -120.2076149402627294, 17.50000000000000000 ) ) ;
#12028 = DIRECTION ( 'NONE',  ( 1.000000000000000000, 0.000000000000000000, 0.000000000000000000 ) ) ;
#12029 = CARTESIAN_POINT ( 'NONE',  ( -99.99999999999998579, -100.7735026918963115, 17.50000000000000000 ) ) ;
#12030 = CARTESIAN_POINT ( 'NONE',  ( -1.846868145590734756, -24.37500000136559564, -4.458734125000000326 ) ) ;
#12031 = CARTESIAN_POINT ( 'NONE',  ( -41.99999999999978684, -11.00000000000000178, -3.500000000000000888 ) ) ;
#12032 = EDGE_CURVE ( 'NONE', #10782, #9986, #13443, .T. ) ;
#12033 = AXIS2_PLACEMENT_3D ( 'NONE', #4889, #9814, #14743 ) ;
#12034 = DIRECTION ( 'NONE',  ( 0.000000000000000000, 0.5000000000000011102, 0.8660254037844380415 ) ) ;
#12035 = EDGE_CURVE ( 'NONE', #14017, #5812, #13056, .T. ) ;
#12036 = CARTESIAN_POINT ( 'NONE',  ( 35.00000000000000000, 50.00000000000000000, 0.000000000000000000 ) ) ;
#12037 = DIRECTION ( 'NONE',  ( 0.000000000000000000, 1.000000000000000000, -0.000000000000000000 ) ) ;
#12038 = ORIENTED_EDGE ( 'NONE', *, *, #15692, .T. ) ;
#12039 = PRODUCT_DEFINITION_FORMATION_WITH_SPECIFIED_SOURCE ( 'ANY', '', #10551, .NOT_KNOWN. ) ;
#12040 = AXIS2_PLACEMENT_3D ( 'NONE', #5261, #4043, #3888 ) ;
#12041 = ORIENTED_EDGE ( 'NONE', *, *, #8396, .T. ) ;
#12042 = CARTESIAN_POINT ( 'NONE',  ( -6.439685834477302251, 4.942299687812321984, -7.659344964962857993 ) ) ;
#12043 = ORIENTED_EDGE ( 'NONE', *, *, #14547, .T. ) ;
#12044 = AXIS2_PLACEMENT_3D ( 'NONE', #5526, #14254, #2851 ) ;
#12045 = CARTESIAN_POINT ( 'NONE',  ( -2.071067811865489272, -26.68750000000000000, -4.999999999999985789 ) ) ;
#12046 = DIRECTION ( 'NONE',  ( 0.000000000000000000, 0.000000000000000000, 1.000000000000000000 ) ) ;
#12047 = ADVANCED_FACE ( 'NONE', ( #15668 ), #7416, .T. ) ;
#12048 = CARTESIAN_POINT ( 'NONE',  ( -3.753672977998669946, -3.033343224707661712, 0.2500000013655933606 ) ) ;
#12049 = DIRECTION ( 'NONE',  ( 0.5000000000000041078, 0.000000000000000000, -0.8660254037844364872 ) ) ;
#12050 = EDGE_CURVE ( 'NONE', #1886, #7410, #11765, .T. ) ;
#12051 = CARTESIAN_POINT ( 'NONE',  ( -3.916244202832140253, 2.131511515620587272, -0.1874999986344084990 ) ) ;
#12052 = VECTOR ( 'NONE', #12987, 1000.000000000000114 ) ;
#12053 = EDGE_LOOP ( 'NONE', ( #10409, #9825, #11375, #9322 ) ) ;
#12054 = CIRCLE ( 'NONE', #6408, 2.500000000000909495 ) ;
#12055 = FILL_AREA_STYLE_COLOUR ( '', #11476 ) ;
#12056 = ORIENTED_EDGE ( 'NONE', *, *, #625, .F. ) ;
#12057 = DIRECTION ( 'NONE',  ( -1.000000000000000000, 0.000000000000000000, -0.000000000000000000 ) ) ;
#12058 = ORIENTED_EDGE ( 'NONE', *, *, #1161, .T. ) ;
#12059 = AXIS2_PLACEMENT_3D ( 'NONE', #6272, #11354, #11427 ) ;
#12060 = ORIENTED_EDGE ( 'NONE', *, *, #6241, .F. ) ;
#12061 = CARTESIAN_POINT ( 'NONE',  ( 4.276409079477644148, 1.261996585732577891, -1.562499998634406140 ) ) ;
#12062 = CARTESIAN_POINT ( 'NONE',  ( -99.99999999999998579, -100.7735026918963115, 17.50000000000000000 ) ) ;
#12063 = PRESENTATION_LAYER_ASSIGNMENT (  '', '', ( #9256 ) ) ;
#12064 = B_SPLINE_CURVE_WITH_KNOTS ( 'NONE', 3,
 ( #10621, #682, #5607, #10547, #9328, #7228, #3570, #14890, #9951, #2193, #6246, #1301, #7463, #4943, #12284, #103 ),
 .UNSPECIFIED., .F., .F.,
 ( 4, 2, 2, 2, 2, 2, 2, 4 ),
 ( 6.534274128967059438E-16, 0.0003988053453845139722, 0.0007976106907683744958, 0.001196416036152234911, 0.001595221381536094350, 0.002392832072303797616, 0.002791637417687638408, 0.003190442763071479632 ),
 .UNSPECIFIED. ) ;
#12065 = COLOUR_RGB ( '', 0.08235294, 0.09019608, 0.10196078) ;
#12066 = DIRECTION ( 'NONE',  ( 1.000000000000000000, 0.000000000000000000, -0.000000000000000000 ) ) ;
#12067 = LINE ( 'NONE', #1083, #11905 ) ;
#12068 = EDGE_CURVE ( 'NONE', #11995, #2056, #14365, .T. ) ;
#12069 = DIRECTION ( 'NONE',  ( -0.000000000000000000, 1.000000000000000000, -0.000000000000000000 ) ) ;
#12070 = AXIS2_PLACEMENT_3D ( 'NONE', #8529, #2287, #7305 ) ;
#12071 = CARTESIAN_POINT ( 'NONE',  ( 2.390265326283148806, 4.391654775818395251, 0.2500000027311835571 ) ) ;
#12072 = PLANE ( 'NONE',  #5910 ) ;
#12073 =( NAMED_UNIT ( * ) SI_UNIT ( $, .STERADIAN. ) SOLID_ANGLE_UNIT ( ) );
#12074 = CARTESIAN_POINT ( 'NONE',  ( -3.152801135295367096, -29.31250000136559564, -3.152801135295367541 ) ) ;
#12075 = CARTESIAN_POINT ( 'NONE',  ( 4.799145180956616130, -0.5093500532425063732, -3.374999998634407472 ) ) ;
#12076 = ORIENTED_EDGE ( 'NONE', *, *, #5448, .F. ) ;
#12077 = CARTESIAN_POINT ( 'NONE',  ( 2.621328321947449691, 7.606199919102465401, -7.633618187056574911 ) ) ;
#12078 = ORIENTED_EDGE ( 'NONE', *, *, #294, .F. ) ;
#12079 = ORIENTED_EDGE ( 'NONE', *, *, #6442, .F. ) ;
#12080 = CIRCLE ( 'NONE', #5149, 2.649999999999992806 ) ;
#12081 = EDGE_LOOP ( 'NONE', ( #9898, #130, #539, #15490 ) ) ;
#12082 = CARTESIAN_POINT ( 'NONE',  ( -3.152801135295367985, -27.06250000136559564, 3.152801135295367096 ) ) ;
#12083 = CARTESIAN_POINT ( 'NONE',  ( 19.99999999999956657, -8.786575603324269439E-13, -6.000000000000000000 ) ) ;
#12084 = AXIS2_PLACEMENT_3D ( 'NONE', #11177, #5282, #14092 ) ;
#12085 = CARTESIAN_POINT ( 'NONE',  ( 0.000000000000000000, 0.000000000000000000, -25.03750572909317285 ) ) ;
#12086 = EDGE_CURVE ( 'NONE', #10126, #8371, #426, .T. ) ;
#12087 = DIRECTION ( 'NONE',  ( -1.000000000000000000, 0.000000000000000000, 0.000000000000000000 ) ) ;
#12088 = FACE_OUTER_BOUND ( 'NONE', #4782, .T. ) ;
#12089 = VECTOR ( 'NONE', #9782, 1000.000000000000114 ) ;
#12090 = AXIS2_PLACEMENT_3D ( 'NONE', #12340, #620, #2562 ) ;
#12091 = DIRECTION ( 'NONE',  ( 1.000000000000000000, 0.000000000000000000, 0.000000000000000000 ) ) ;
#12092 = CARTESIAN_POINT ( 'NONE',  ( -2.390265326283148806, -4.391654775818394363, -0.3750000000000003331 ) ) ;
#12093 = CARTESIAN_POINT ( 'NONE',  ( 2.390265326283148806, 4.391654775818395251, -3.875000000000000000 ) ) ;
#12094 = CARTESIAN_POINT ( 'NONE',  ( -5.000000000000000888, -27.56250000000000000, -2.071067811865475949 ) ) ;
#12095 = CARTESIAN_POINT ( 'NONE',  ( -2.071067811865475061, -21.81250000273118772, -5.000000000000000888 ) ) ;
#12096 =( BOUNDED_CURVE ( )  B_SPLINE_CURVE ( 2, ( #2446, #4652, #8694, #2304, #1086, #9818, #4728, #49, #2216 ),
 .UNSPECIFIED., .F., .F. ) 
 B_SPLINE_CURVE_WITH_KNOTS ( ( 3, 2, 2, 2, 3 ),
 ( 0.7249999999999999778, 0.7375000000000000444, 0.7500000000000000000, 0.7624999999999999556, 0.7750000000000000222 ),
 .UNSPECIFIED. ) 
 CURVE ( )  GEOMETRIC_REPRESENTATION_ITEM ( )  RATIONAL_B_SPLINE_CURVE ( ( 1.000000000000000000, 0.9238795325112867385, 1.000000000000000000, 0.9238795325112867385, 1.000000000000000000, 0.9238795325112867385, 1.000000000000000000, 0.9238795325112867385, 1.000000000000000000 ) ) 
 REPRESENTATION_ITEM ( '' )  );
#12097 = CARTESIAN_POINT ( 'NONE',  ( -3.753672977998669946, -3.033343224707661712, 1.000000001365594082 ) ) ;
#12098 = ORIENTED_EDGE ( 'NONE', *, *, #1782, .F. ) ;
#12099 = FACE_OUTER_BOUND ( 'NONE', #9228, .T. ) ;
#12100 = B_SPLINE_CURVE_WITH_KNOTS ( 'NONE', 3,
 ( #12950, #1887, #5692, #4403, #7971, #12875, #5532, #10468, #15400, #10628 ),
 .UNSPECIFIED., .F., .F.,
 ( 4, 2, 2, 2, 4 ),
 ( 0.01051144076094936118, 0.01162027323572612306, 0.01272910571050288493, 0.01383793818527964507, 0.01494677066005640695 ),
 .UNSPECIFIED. ) ;
#12101 = VERTEX_POINT ( 'NONE', #9749 ) ;
#12102 = ORIENTED_EDGE ( 'NONE', *, *, #9664, .T. ) ;
#12103 = CARTESIAN_POINT ( 'NONE',  ( -4.000000000000000000, 2.309401076758498483, -3.433295621305379353 ) ) ;
#12104 = CARTESIAN_POINT ( 'NONE',  ( 4.458734125000000326, -27.37500000136559564, -1.846868145590734978 ) ) ;
#12105 = DIRECTION ( 'NONE',  ( 0.000000000000000000, -1.000000000000000000, 0.000000000000000000 ) ) ;
#12106 = VERTEX_POINT ( 'NONE', #7259 ) ;
#12108 = VECTOR ( 'NONE', #9963, 1000.000000000000000 ) ;
#12107 = CYLINDRICAL_SURFACE ( 'NONE', #162, 2.649999999999992806 ) ;
#12109 = ADVANCED_FACE ( 'NONE', ( #4665 ), #7183, .T. ) ;
#12110 = ADVANCED_FACE ( 'NONE', ( #14686 ), #8554, .F. ) ;
#12111 = CARTESIAN_POINT ( 'NONE',  ( -6.765421556309547668E-13, 37.00000000000000000, 67.49999999999930367 ) ) ;
#12112 = CARTESIAN_POINT ( 'NONE',  ( -44.43375672972994295, -5.000000000000000000, -20.00000000000000355 ) ) ;
#12113 = FACE_OUTER_BOUND ( 'NONE', #14658, .T. ) ;
#12114 = CARTESIAN_POINT ( 'NONE',  ( 2.730187237215162345E-16, -22.43750000136559564, -4.458734124999999437 ) ) ;
#12115 = FACE_OUTER_BOUND ( 'NONE', #4997, .T. ) ;
#12116 = CARTESIAN_POINT ( 'NONE',  ( 2.500000000000000000, 2.357898499370433054, -1.951563910473907981E-15 ) ) ;
#12117 = CARTESIAN_POINT ( 'NONE',  ( 5.000000000000000000, -31.06250000000000000, 2.071067811865478614 ) ) ;
#12118 = CARTESIAN_POINT ( 'NONE',  ( 1.415196051561583790, -4.795541693661363958, -6.124999997268814944 ) ) ;
#12119 = CARTESIAN_POINT ( 'NONE',  ( -19.99999999999956657, -11.00000000000000178, 8.786575603324269439E-13 ) ) ;
#12120 = ORIENTED_EDGE ( 'NONE', *, *, #9564, .T. ) ;
#12121 = SHAPE_DEFINITION_REPRESENTATION ( #6804, #4176 ) ;
#12122 = EDGE_LOOP ( 'NONE', ( #8826, #5235, #13372, #14859 ) ) ;
#12123 = FACE_OUTER_BOUND ( 'NONE', #6679, .T. ) ;
#12124 = ORIENTED_EDGE ( 'NONE', *, *, #3180, .T. ) ;
#12125 = EDGE_CURVE ( 'NONE', #9076, #2433, #8115, .T. ) ;
#12126 = CARTESIAN_POINT ( 'NONE',  ( 7.500000000000000000, 4.330127018922190096, -9.999999999999998224 ) ) ;
#12127 = DIRECTION ( 'NONE',  ( 0.000000000000000000, 0.000000000000000000, 1.000000000000000000 ) ) ;
#12128 = CARTESIAN_POINT ( 'NONE',  ( 5.000000000000000000, -28.06250000000000000, 2.071067811865478614 ) ) ;
#12129 = CARTESIAN_POINT ( 'NONE',  ( -6.754399735117222262E-13, 55.00000000000000000, 67.49999999999931788 ) ) ;
#12130 = CARTESIAN_POINT ( 'NONE',  ( 4.799145180956616130, -0.5093500532425063732, 0.3750000013655915843 ) ) ;
#12131 = CARTESIAN_POINT ( 'NONE',  ( 1.391697335622810172, 4.043246145443375461, -3.503898532754365913 ) ) ;
#12132 = ORIENTED_EDGE ( 'NONE', *, *, #14027, .F. ) ;
#12133 = DIRECTION ( 'NONE',  ( 0.000000000000000000, 0.4999999999999993894, -0.8660254037844389297 ) ) ;
#12134 =( NAMED_UNIT ( * ) SI_UNIT ( $, .STERADIAN. ) SOLID_ANGLE_UNIT ( ) );
#12135 = ORIENTED_EDGE ( 'NONE', *, *, #13824, .T. ) ;
#12136 = CARTESIAN_POINT ( 'NONE',  ( 4.000000000000000888, 0.8228435280416209752, -3.430609588141487976 ) ) ;
#12137 = ORIENTED_EDGE ( 'NONE', *, *, #14112, .T. ) ;
#12138 = EDGE_LOOP ( 'NONE', ( #4501, #2704, #7277, #7940, #15076, #75, #5539, #2050, #1327, #11666, #8409, #12292 ) ) ;
#12139 = CARTESIAN_POINT ( 'NONE',  ( -3.033343224707664820, 3.753672977998667726, -4.249999998634407028 ) ) ;
#12140 = ADVANCED_FACE ( 'NONE', ( #4904 ), #12001, .T. ) ;
#12141 = EDGE_CURVE ( 'NONE', #13521, #2457, #3441, .T. ) ;
#12142 = EDGE_CURVE ( 'NONE', #11174, #3781, #8710, .T. ) ;
#12143 = EDGE_CURVE ( 'NONE', #5100, #2789, #14090, .T. ) ;
#12144 = CARTESIAN_POINT ( 'NONE',  ( -2.071067811865492381, -29.31250000000000000, 4.999999999999985789 ) ) ;
#12145 = CARTESIAN_POINT ( 'NONE',  ( -7.897850199329722543, 1.533397866934075759, -7.634054012537968781 ) ) ;
#12146 = FACE_OUTER_BOUND ( 'NONE', #15023, .T. ) ;
#12147 = CARTESIAN_POINT ( 'NONE',  ( -2.071067811865456854, -29.43750000273118062, 5.000000000000021316 ) ) ;
#12148 = CARTESIAN_POINT ( 'NONE',  ( -4.795541693661363958, -1.415196051561583790, -1.374999997268814500 ) ) ;
#12149 = PRESENTATION_STYLE_ASSIGNMENT (( #4811 ) ) ;
#12150 = SURFACE_STYLE_FILL_AREA ( #12286 ) ;
#12151 = CARTESIAN_POINT ( 'NONE',  ( 1.846868145590735200, -27.50000000136559564, -4.458734124999999437 ) ) ;
#12152 = CARTESIAN_POINT ( 'NONE',  ( 3.033343224707661712, -3.753672977998669946, -3.499999998634410137 ) ) ;
#12153 = DIRECTION ( 'NONE',  ( 0.000000000000000000, 0.000000000000000000, 1.000000000000000000 ) ) ;
#12154 = ORIENTED_EDGE ( 'NONE', *, *, #11164, .T. ) ;
#12155 = ORIENTED_EDGE ( 'NONE', *, *, #2599, .F. ) ;
#12156 = SURFACE_STYLE_FILL_AREA ( #9437 ) ;
#12157 = ORIENTED_EDGE ( 'NONE', *, *, #2547, .T. ) ;
#12158 = CARTESIAN_POINT ( 'NONE',  ( -3.152801135295367985, -24.06250000136559564, 3.152801135295367096 ) ) ;
#12159 = CARTESIAN_POINT ( 'NONE',  ( -5.000000000000000888, -23.68750000273119127, -2.071067811865475949 ) ) ;
#12160 = EDGE_CURVE ( 'NONE', #1955, #13141, #10754, .T. ) ;
#12161 = DIRECTION ( 'NONE',  ( -0.000000000000000000, 1.000000000000000000, -0.000000000000000000 ) ) ;
#12162 = CARTESIAN_POINT ( 'NONE',  ( 0.000000000000000000, -20.00000000000000000, 0.000000000000000000 ) ) ;
#12163 = DIRECTION ( 'NONE',  ( 0.000000000000000000, 0.000000000000000000, 1.000000000000000000 ) ) ;
#12164 = DIRECTION ( 'NONE',  ( -0.000000000000000000, 1.000000000000000000, -0.000000000000000000 ) ) ;
#12165 = CARTESIAN_POINT ( 'NONE',  ( 5.381735091635035495, -0.5711823568785978633, -3.062500000000001776 ) ) ;
#12166 = CARTESIAN_POINT ( 'NONE',  ( -6.259644161404860030E-16, -4.618802153517027165, -5.000000000000000000 ) ) ;
#12167 = CARTESIAN_POINT ( 'NONE',  ( 2.286513180745818108, -4.371196073312955122, -0.05185736845305202042 ) ) ;
#12168 = CARTESIAN_POINT ( 'NONE',  ( 3.152801135295366208, -26.56250000136559564, 3.152801135295367985 ) ) ;
#12169 = CARTESIAN_POINT ( 'NONE',  ( 3.916244202832140253, -2.131511515620588160, -1.687499998634406362 ) ) ;
#12170 = ORIENTED_EDGE ( 'NONE', *, *, #905, .T. ) ;
#12171 = CARTESIAN_POINT ( 'NONE',  ( -31.74999999999995737, 3.061616997868384127E-16, -2.500000000000000888 ) ) ;
#12172 = EDGE_LOOP ( 'NONE', ( #109, #11882 ) ) ;
#12173 = EDGE_LOOP ( 'NONE', ( #13706, #10262, #1150, #4868 ) ) ;
#12174 = CARTESIAN_POINT ( 'NONE',  ( -4.000000000000000000, -7.806255641895631925E-15, -3.142992957459232350 ) ) ;
#12175 = CARTESIAN_POINT ( 'NONE',  ( 4.458734124999999437, -25.50000000136559919, 1.846868145590737864 ) ) ;
#12176 = CARTESIAN_POINT ( 'NONE',  ( -115.0000000000000142, -10.00000000000000888, -7.500000000000000000 ) ) ;
#12177 = ORIENTED_EDGE ( 'NONE', *, *, #13846, .F. ) ;
#12178 = AXIS2_PLACEMENT_3D ( 'NONE', #8737, #1360, #3547 ) ;
#12179 = LINE ( 'NONE', #8421, #4017 ) ;
#12180 = AXIS2_PLACEMENT_3D ( 'NONE', #14274, #10641, #1745 ) ;
#12181 = CARTESIAN_POINT ( 'NONE',  ( 5.000000000000000000, -22.06250000000000000, 2.071067811865478614 ) ) ;
#12182 = DIRECTION ( 'NONE',  ( 0.000000000000000000, 0.000000000000000000, 1.000000000000000000 ) ) ;
#12183 = FACE_OUTER_BOUND ( 'NONE', #817, .T. ) ;
#12184 = CARTESIAN_POINT ( 'NONE',  ( -1.846868145590737420, -25.00000000136559564, 4.458734124999999437 ) ) ;
#12185 = CARTESIAN_POINT ( 'NONE',  ( 19.99999999999956657, -8.786575603324269439E-13, 0.000000000000000000 ) ) ;
#12186 = CARTESIAN_POINT ( 'NONE',  ( -1.240299975428134203E-15, -4.736529461165891242, -3.681130640444276292 ) ) ;
#12187 = CARTESIAN_POINT ( 'NONE',  ( -9.184850993605147944E-16, -31.25000000000000000, 5.000000000000000888 ) ) ;
#12188 = LINE ( 'NONE', #9938, #14012 ) ;
#12189 = AXIS2_PLACEMENT_3D ( 'NONE', #5983, #8653, #8578 ) ;
#12190 = DIRECTION ( 'NONE',  ( 0.000000000000000000, 0.000000000000000000, 1.000000000000000000 ) ) ;
#12191 = EDGE_CURVE ( 'NONE', #4347, #11118, #947, .T. ) ;
#12192 = CARTESIAN_POINT ( 'NONE',  ( -15.99999999999979217, -11.00000000000000178, -1.500000000000001110 ) ) ;
#12193 = AXIS2_PLACEMENT_3D ( 'NONE', #13315, #9690, #2257 ) ;
#12195 = ADVANCED_FACE ( 'NONE', ( #7822, #1416, #8949, #6520, #5301 ), #1582, .T. ) ;
#12194 = ORIENTED_EDGE ( 'NONE', *, *, #1593, .T. ) ;
#12196 = ORIENTED_EDGE ( 'NONE', *, *, #15439, .F. ) ;
#12197 = DIRECTION ( 'NONE',  ( 0.000000000000000000, 0.000000000000000000, 1.000000000000000000 ) ) ;
#12198 = ORIENTED_EDGE ( 'NONE', *, *, #10043, .T. ) ;
#12199 = CYLINDRICAL_SURFACE ( 'NONE', #10255, 25.00000000000000000 ) ;
#12200 = LINE ( 'NONE', #11010, #11576 ) ;
#12201 = CARTESIAN_POINT ( 'NONE',  ( 1.261996585732578113, -4.276409079477644148, 1.437500001365592972 ) ) ;
#12202 = DIRECTION ( 'NONE',  ( -1.000000000000000000, 0.000000000000000000, 0.000000000000000000 ) ) ;
#12203 = PRODUCT_DEFINITION_SHAPE ( 'NONE', 'NONE',  #15973 ) ;
#12204 = CARTESIAN_POINT ( 'NONE',  ( 4.799145180956616130, -0.5093500532425063732, -1.624999998634406362 ) ) ;
#12205 = CARTESIAN_POINT ( 'NONE',  ( 0.000000000000000000, -2.357898499370432610, 3.252606517456513302E-15 ) ) ;
#12206 = ADVANCED_FACE ( 'NONE', ( #9903 ), #13862, .F. ) ;
#12207 = SURFACE_SIDE_STYLE ('',( #8527 ) ) ;
#12208 = EDGE_CURVE ( 'NONE', #15584, #6071, #13311, .T. ) ;
#12209 = CARTESIAN_POINT ( 'NONE',  ( -124.9999999999999716, -10.00000000000001066, -7.500000000000000000 ) ) ;
#12210 = ORIENTED_EDGE ( 'NONE', *, *, #5138, .F. ) ;
#12211 = CARTESIAN_POINT ( 'NONE',  ( 4.203935335434060505, 1.640780671294165272, -3.598452447879202598 ) ) ;
#12212 = VERTEX_POINT ( 'NONE', #2545 ) ;
#12213 =( GEOMETRIC_REPRESENTATION_CONTEXT ( 3 ) GLOBAL_UNCERTAINTY_ASSIGNED_CONTEXT ( ( #9023 ) ) GLOBAL_UNIT_ASSIGNED_CONTEXT ( ( #15383, #6812, #9473 ) ) REPRESENTATION_CONTEXT ( 'NONE', 'WORKASPACE' ) );
#12214 = ORIENTED_EDGE ( 'NONE', *, *, #10856, .T. ) ;
#12215 = CARTESIAN_POINT ( 'NONE',  ( 3.033343224707661712, -3.753672977998669502, -3.749999998634410137 ) ) ;
#12216 = DIRECTION ( 'NONE',  ( 0.000000000000000000, -0.000000000000000000, -1.000000000000000000 ) ) ;
#12217 = CARTESIAN_POINT ( 'NONE',  ( 2.500000000000000000, -2.629050547790028551E-15, -2.041999999999999815 ) ) ;
#12218 = DIRECTION ( 'NONE',  ( -0.000000000000000000, 1.000000000000000000, -0.000000000000000000 ) ) ;
#12219 = FACE_OUTER_BOUND ( 'NONE', #11592, .T. ) ;
#12220 = CARTESIAN_POINT ( 'NONE',  ( 0.000000000000000000, -1.178949249685218303, -2.041999999999998039 ) ) ;
#12221 = CARTESIAN_POINT ( 'NONE',  ( 1.415196051561583790, -4.795541693661363958, -1.124999997268814278 ) ) ;
#12222 = EDGE_CURVE ( 'NONE', #6666, #79, #3764, .T. ) ;
#12223 = SURFACE_STYLE_USAGE ( .BOTH. , #8312 ) ;
#12224 = CARTESIAN_POINT ( 'NONE',  ( -1.846868145590734756, -24.37500000136559564, -4.458734124999999437 ) ) ;
#12225 = EDGE_CURVE ( 'NONE', #6165, #1597, #11525, .T. ) ;
#12226 = VECTOR ( 'NONE', #2546, 1000.000000000000000 ) ;
#12227 = CARTESIAN_POINT ( 'NONE',  ( -4.458734124999999437, -22.93750000136559564, -5.460374474430324690E-16 ) ) ;
#12228 = CARTESIAN_POINT ( 'NONE',  ( 2.131511515620586383, 3.916244202832140253, -6.187499998634407028 ) ) ;
#12229 = CARTESIAN_POINT ( 'NONE',  ( 33.48631561299828974, -4.999999999999997335, 14.00000000000001243 ) ) ;
#12230 = B_SPLINE_CURVE_WITH_KNOTS ( 'NONE', 3,
 ( #11602, #10642, #3198, #9349 ),
 .UNSPECIFIED., .F., .F.,
 ( 4, 4 ),
 ( 1.661095388496746134E-17, 0.0005803541179376217390 ),
 .UNSPECIFIED. ) ;
#12231 = ORIENTED_EDGE ( 'NONE', *, *, #12522, .F. ) ;
#12232 = EDGE_LOOP ( 'NONE', ( #11191, #14946, #6727, #3739, #14683, #10955, #1370 ) ) ;
#12233 = DIRECTION ( 'NONE',  ( 0.000000000000000000, 0.000000000000000000, 1.000000000000000000 ) ) ;
#12234 = EDGE_LOOP ( 'NONE', ( #10975, #8532, #2327, #14903 ) ) ;
#12235 = CARTESIAN_POINT ( 'NONE',  ( -1.846868145590737420, -24.00000000136559564, 4.458734124999999437 ) ) ;
#12236 = DIRECTION ( 'NONE',  ( -0.000000000000000000, -0.000000000000000000, 1.000000000000000000 ) ) ;
#12237 = TOROIDAL_SURFACE ( 'NONE', #5285, 4.000000000000000000, 0.2500000000000000000 ) ;
#12238 = PLANE ( 'NONE',  #9925 ) ;
#12239 = CIRCLE ( 'NONE', #5291, 2.649999999999992806 ) ;
#12240 = CARTESIAN_POINT ( 'NONE',  ( -124.9999999999999858, -115.2072594216369907, -7.500000000000000000 ) ) ;
#12241 = CARTESIAN_POINT ( 'NONE',  ( -99.99999999999998579, -10.00000000000000888, -17.50000000000000000 ) ) ;
#12242 = CARTESIAN_POINT ( 'NONE',  ( -3.535533905932738641, -22.37500000000000000, 3.535533905932737309 ) ) ;
#12243 = CARTESIAN_POINT ( 'NONE',  ( -1.415196051561583790, 4.795541693661363958, -0.7500000000000006661 ) ) ;
#12244 = CARTESIAN_POINT ( 'NONE',  ( -44.99999999999999289, -13.00000000000000178, -3.999999999999170885 ) ) ;
#12245 = CARTESIAN_POINT ( 'NONE',  ( 0.7619918569178352197, -4.833934400323800951, -0.07953229779526811705 ) ) ;
#12246 = CARTESIAN_POINT ( 'NONE',  ( -1.846868145590734756, -28.12500000136559564, -4.458734125000000326 ) ) ;
#12247 = PRESENTATION_LAYER_ASSIGNMENT (  '', '', ( #3998 ) ) ;
#12248 = ADVANCED_FACE ( 'NONE', ( #2793 ), #6282, .T. ) ;
#12249 = CARTESIAN_POINT ( 'NONE',  ( 0.5093500532425063732, 4.799145180956616130, -3.374999998634407472 ) ) ;
#12250 = ORIENTED_EDGE ( 'NONE', *, *, #10043, .F. ) ;
#12251 = VECTOR ( 'NONE', #13475, 1000.000000000000000 ) ;
#12252 = DIRECTION ( 'NONE',  ( 0.000000000000000000, 0.000000000000000000, 1.000000000000000000 ) ) ;
#12253 = ORIENTED_EDGE ( 'NONE', *, *, #9852, .T. ) ;
#12254 = ORIENTED_EDGE ( 'NONE', *, *, #11708, .T. ) ;
#12256 = CARTESIAN_POINT ( 'NONE',  ( -90.00000000000000000, -94.99999999999995737, -13.35786437626905077 ) ) ;
#12255 = AXIS2_PLACEMENT_3D ( 'NONE', #3013, #13997, #6904 ) ;
#12257 = CARTESIAN_POINT ( 'NONE',  ( -1.846868145590734756, -25.12500000136559564, -4.458734125000000326 ) ) ;
#12258 = CARTESIAN_POINT ( 'NONE',  ( 4.535975386569504053, 1.338596318647080397, -8.718749997951611874 ) ) ;
#12259 = VERTEX_POINT ( 'NONE', #10157 ) ;
#12260 = DIRECTION ( 'NONE',  ( -0.000000000000000000, 1.000000000000000000, -0.000000000000000000 ) ) ;
#12261 = VECTOR ( 'NONE', #12471, 1000.000000000000000 ) ;
#12262 = DIRECTION ( 'NONE',  ( 0.000000000000000000, 0.000000000000000000, 1.000000000000000000 ) ) ;
#12263 = DIRECTION ( 'NONE',  ( 1.000000000000000000, 0.000000000000000000, 0.000000000000000000 ) ) ;
#12264 = CARTESIAN_POINT ( 'NONE',  ( 0.000000000000000000, 37.00000000000000000, -60.00000000000000000 ) ) ;
#12265 = AXIS2_PLACEMENT_3D ( 'NONE', #4996, #11069, #6056 ) ;
#12266 = CARTESIAN_POINT ( 'NONE',  ( 2.730187237215162345E-16, -24.43750000136559564, -4.458734124999999437 ) ) ;
#12267 = AXIS2_PLACEMENT_3D ( 'NONE', #4356, #2000, #3299 ) ;
#12268 = DIRECTION ( 'NONE',  ( 0.000000000000000000, 0.000000000000000000, 1.000000000000000000 ) ) ;
#12269 = CARTESIAN_POINT ( 'NONE',  ( -0.5711823568785977523, -5.381735091635034607, -1.187499997268815610 ) ) ;
#12270 = CARTESIAN_POINT ( 'NONE',  ( 2.071067811865475505, -29.93750000273118417, -5.000000000000000888 ) ) ;
#12271 = ADVANCED_FACE ( 'NONE', ( #3997 ), #13772, .F. ) ;
#12272 = CARTESIAN_POINT ( 'NONE',  ( -4.209348295687703079, -3.401574460001763445, -6.312499997268814056 ) ) ;
#12273 = CARTESIAN_POINT ( 'NONE',  ( 2.730187237215162345E-16, -31.18750000136559564, -4.458734124999999437 ) ) ;
#12274 = FILL_AREA_STYLE_COLOUR ( '', #11478 ) ;
#12275 = ORIENTED_EDGE ( 'NONE', *, *, #4930, .T. ) ;
#12276 =( GEOMETRIC_REPRESENTATION_CONTEXT ( 3 ) GLOBAL_UNCERTAINTY_ASSIGNED_CONTEXT ( ( #6103 ) ) GLOBAL_UNIT_ASSIGNED_CONTEXT ( ( #10053, #6659, #7954 ) ) REPRESENTATION_CONTEXT ( 'NONE', 'WORKASPACE' ) );
#12277 = ORIENTED_EDGE ( 'NONE', *, *, #4461, .F. ) ;
#12278 = CARTESIAN_POINT ( 'NONE',  ( -0.3208286057739654917, 4.433571671609680465, -0.3503314178412548774 ) ) ;
#12279 = AXIS2_PLACEMENT_3D ( 'NONE', #2314, #15752, #8475 ) ;
#12280 = ORIENTED_EDGE ( 'NONE', *, *, #13644, .T. ) ;
#12281 = DIRECTION ( 'NONE',  ( 0.000000000000000000, 0.000000000000000000, 1.000000000000000000 ) ) ;
#12282 = EDGE_CURVE ( 'NONE', #4793, #8839, #5060, .T. ) ;
#12283 = CIRCLE ( 'NONE', #7682, 3.499999999999999556 ) ;
#12284 = CARTESIAN_POINT ( 'NONE',  ( 40.89008552033507726, -3.000000000000000444, 27.08056972037525867 ) ) ;
#12285 = CARTESIAN_POINT ( 'NONE',  ( 4.276409079477644148, 1.261996585732577891, -2.312499998634407028 ) ) ;
#12286 = FILL_AREA_STYLE ('',( #862 ) ) ;
#12287 = DIRECTION ( 'NONE',  ( 6.123233995736766036E-17, -1.000000000000000000, 0.000000000000000000 ) ) ;
#12288 = AXIS2_PLACEMENT_3D ( 'NONE', #2498, #98, #2059 ) ;
#12289 = CARTESIAN_POINT ( 'NONE',  ( -1.261996585732579224, 4.276409079477648589, -3.312499998634407916 ) ) ;
#12290 = DIRECTION ( 'NONE',  ( -0.000000000000000000, -1.000000000000000000, -0.000000000000000000 ) ) ;
#12291 = LINE ( 'NONE', #2358, #9751 ) ;
#12292 = ORIENTED_EDGE ( 'NONE', *, *, #8722, .T. ) ;
#12293 = CARTESIAN_POINT ( 'NONE',  ( -28.86751345948130165, -35.00000000000000000, 17.99999999999999645 ) ) ;
#12294 = AXIS2_PLACEMENT_3D ( 'NONE', #4744, #4906, #13378 ) ;
#12295 = DIRECTION ( 'NONE',  ( 0.000000000000000000, 0.000000000000000000, 1.000000000000000000 ) ) ;
#12296 = EDGE_LOOP ( 'NONE', ( #483, #6134, #11665, #4445 ) ) ;
#12297 = ITEM_DEFINED_TRANSFORMATION ( 'NONE', 'NONE', #9165,  #3223 ) ;
#12298 = CARTESIAN_POINT ( 'NONE',  ( -4.276409079477644148, -1.261996585732578335, -3.062499998634407472 ) ) ;
#12299 = CARTESIAN_POINT ( 'NONE',  ( 5.000000000000000888, 0.000000000000000000, 0.000000000000000000 ) ) ;
#12300 = ADVANCED_FACE ( 'NONE', ( #6363 ), #12477, .T. ) ;
#12301 = EDGE_CURVE ( 'NONE', #5616, #11530, #7147, .T. ) ;
#12302 = CARTESIAN_POINT ( 'NONE',  ( -3.535533905932737309, -29.62500000000000355, -3.535533905932738197 ) ) ;
#12303 = FACE_OUTER_BOUND ( 'NONE', #594, .T. ) ;
#12304 = CARTESIAN_POINT ( 'NONE',  ( 4.999999999999849010, -1.272547481429013416, -2.086597482644648949 ) ) ;
#12305 = FACE_OUTER_BOUND ( 'NONE', #13538, .T. ) ;
#12306 = CARTESIAN_POINT ( 'NONE',  ( -0.5711823568785978633, -5.381735091635035495, 0.8125000027311823914 ) ) ;
#12307 =( NAMED_UNIT ( * ) SI_UNIT ( $, .STERADIAN. ) SOLID_ANGLE_UNIT ( ) );
#12308 = CARTESIAN_POINT ( 'NONE',  ( -9.184850993605147944E-16, -28.37500000273118772, 5.000000000000000000 ) ) ;
#12309 = CARTESIAN_POINT ( 'NONE',  ( -4.458734125000000326, -27.12500000136559564, 1.846868145590734089 ) ) ;
#12310 = CARTESIAN_POINT ( 'NONE',  ( -1.846868145590734756, -23.12500000136559564, -4.458734124999999437 ) ) ;
#12311 = CARTESIAN_POINT ( 'NONE',  ( -3.033343224707664376, 3.753672977998667726, -5.999999998634407916 ) ) ;
#12312 = AXIS2_PLACEMENT_3D ( 'NONE', #10915, #14403, #5828 ) ;
#12313 = VECTOR ( 'NONE', #2284, 1000.000000000000000 ) ;
#12314 = CARTESIAN_POINT ( 'NONE',  ( 1.567478505476134606E-15, 4.618802153517012066, -3.433295621305382905 ) ) ;
#12315 = EDGE_LOOP ( 'NONE', ( #1020, #14106, #2251 ) ) ;
#12316 = VERTEX_POINT ( 'NONE', #2628 ) ;
#12317 = DIRECTION ( 'NONE',  ( -0.5000000000000041078, 0.000000000000000000, 0.8660254037844364872 ) ) ;
#12318 = ORIENTED_EDGE ( 'NONE', *, *, #11853, .F. ) ;
#12319 = CARTESIAN_POINT ( 'NONE',  ( 2.730187237215162345E-16, -22.43750000136559564, -4.458734124999999437 ) ) ;
#12320 = AXIS2_PLACEMENT_3D ( 'NONE', #6872, #5657, #3221 ) ;
#12321 = DIRECTION ( 'NONE',  ( 0.000000000000000000, 0.000000000000000000, -1.000000000000000000 ) ) ;
#12322 = DIRECTION ( 'NONE',  ( 0.000000000000000000, 0.000000000000000000, -1.000000000000000000 ) ) ;
#12323 = EDGE_CURVE ( 'NONE', #869, #6090, #11774, .T. ) ;
#12324 = ADVANCED_FACE ( 'NONE', ( #3120 ), #15253, .F. ) ;
#12325 = AXIS2_PLACEMENT_3D ( 'NONE', #8652, #14545, #15774 ) ;
#12326 = FACE_OUTER_BOUND ( 'NONE', #9304, .T. ) ;
#12327 = FACE_OUTER_BOUND ( 'NONE', #4716, .T. ) ;
#12328 =( BOUNDED_SURFACE ( )  B_SPLINE_SURFACE ( 3, 2, ( 
 ( #13422, #2360, #13670 ),
 ( #2434, #10936, #1074 ),
 ( #3585, #15875, #2514 ),
 ( #3735, #12136, #39 ),
 ( #11020, #9808, #12211 ),
 ( #6336, #12455, #7387 ) ),
 .UNSPECIFIED., .F., .F., .F. ) 
 B_SPLINE_SURFACE_WITH_KNOTS ( ( 4, 2, 4 ),
 ( 3, 3 ),
 ( 0.02027065861071770947, 0.02273072267836921331, 0.02519078674602071716 ),
 ( 0.000000000000000000, 1.000000000000000000 ),
 .UNSPECIFIED. ) 
 GEOMETRIC_REPRESENTATION_ITEM ( )  RATIONAL_B_SPLINE_SURFACE ( (
 ( 1.000000000000000000, 0.8047781708337304885, 1.000000000000000000),
 ( 1.000000000000000000, 0.8123765190705307671, 1.000000000000000000),
 ( 1.000000000000000000, 0.8190656277163975707, 1.000000000000000000),
 ( 1.000000000000000000, 0.8192366903512159348, 1.000000000000000000),
 ( 1.000000000000000000, 0.8126138454302893610, 1.000000000000000000),
 ( 1.000000000000000000, 0.8047712246031417660, 1.000000000000000000) ) ) 
 REPRESENTATION_ITEM ( '' )  SURFACE ( )  );
#12329 = CARTESIAN_POINT ( 'NONE',  ( 0.000000000000000000, -2.357898499370432610, 3.252606517456513302E-15 ) ) ;
#12330 = CARTESIAN_POINT ( 'NONE',  ( -1.415196051561583790, 4.795541693661363958, -2.750000000000002665 ) ) ;
#12331 = LINE ( 'NONE', #10969, #611 ) ;
#12332 = CARTESIAN_POINT ( 'NONE',  ( -3.542429731366778967, -3.193955667491259476, -0.1664247486893449535 ) ) ;
#12333 = CARTESIAN_POINT ( 'NONE',  ( -4.458734124999999437, -27.93750000136559564, -5.460374474430324690E-16 ) ) ;
#12334 = CARTESIAN_POINT ( 'NONE',  ( 4.276409079477644148, 1.261996585732577891, -3.562499998634407916 ) ) ;
#12335 = ORIENTED_EDGE ( 'NONE', *, *, #1176, .F. ) ;
#12336 = DIRECTION ( 'NONE',  ( -0.5000000000000019984, -0.8660254037844375974, 0.000000000000000000 ) ) ;
#12337 = ORIENTED_EDGE ( 'NONE', *, *, #7117, .F. ) ;
#12338 = ORIENTED_EDGE ( 'NONE', *, *, #11925, .T. ) ;
#12339 = VECTOR ( 'NONE', #12388, 1000.000000000000000 ) ;
#12340 = CARTESIAN_POINT ( 'NONE',  ( -31.74999999999995737, 0.000000000000000000, 0.000000000000000000 ) ) ;
#12341 = CIRCLE ( 'NONE', #5390, 2.649999999999992806 ) ;
#12342 = CARTESIAN_POINT ( 'NONE',  ( 1.846868145590735200, -23.25000000136559208, -4.458734125000000326 ) ) ;
#12343 = DIRECTION ( 'NONE',  ( 0.000000000000000000, 0.000000000000000000, 1.000000000000000000 ) ) ;
#12344 = ORIENTED_EDGE ( 'NONE', *, *, #2301, .T. ) ;
#12345 = FACE_OUTER_BOUND ( 'NONE', #12122, .T. ) ;
#12346 = EDGE_CURVE ( 'NONE', #7943, #11470, #4041, .T. ) ;
#12347 = AXIS2_PLACEMENT_3D ( 'NONE', #7826, #6605, #1663 ) ;
#12348 = ADVANCED_FACE ( 'NONE', ( #3034 ), #7981, .F. ) ;
#12349 = AXIS2_PLACEMENT_3D ( 'NONE', #10418, #646, #10592 ) ;
#12350 = EDGE_CURVE ( 'NONE', #8889, #2808, #2224, .T. ) ;
#12351 = CARTESIAN_POINT ( 'NONE',  ( 19.99999999999956657, -8.786575603324269439E-13, -4.500000000000000000 ) ) ;
#12352 = FACE_BOUND ( 'NONE', #8153, .T. ) ;
#12353 = CARTESIAN_POINT ( 'NONE',  ( -1.154700538379222596, 0.000000000000000000, -34.00000000000000000 ) ) ;
#12354 = CARTESIAN_POINT ( 'NONE',  ( 4.458734124999999437, -24.75000000136559564, 1.846868145590737864 ) ) ;
#12355 = CARTESIAN_POINT ( 'NONE',  ( -0.1410422978106123659, 4.700232962125094893, -3.687027686973624707 ) ) ;
#12356 = CARTESIAN_POINT ( 'NONE',  ( -1.240299975428113101E-15, -4.647091401871173311, -3.572172305156514849 ) ) ;
#12357 = CARTESIAN_POINT ( 'NONE',  ( 2.071067811865476394, -28.31250000273118772, 5.000000000000000000 ) ) ;
#12358 = LINE ( 'NONE', #4774, #9132 ) ;
#12359 = CARTESIAN_POINT ( 'NONE',  ( 2.730187237215162345E-16, -29.18750000136559208, -4.458734124999999437 ) ) ;
#12360 = CARTESIAN_POINT ( 'NONE',  ( 0.000000000000000000, -20.00000000000000000, -1.500000000000000000 ) ) ;
#12361 = ORIENTED_EDGE ( 'NONE', *, *, #2364, .T. ) ;
#12362 = VECTOR ( 'NONE', #1216, 999.9999999999998863 ) ;
#12363 = ORIENTED_EDGE ( 'NONE', *, *, #9961, .T. ) ;
#12364 = CARTESIAN_POINT ( 'NONE',  ( -116.3391301858327296, -120.2076149402627294, -7.500000000000000000 ) ) ;
#12365 = EDGE_LOOP ( 'NONE', ( #11003, #12450, #8947, #9028 ) ) ;
#12366 = CARTESIAN_POINT ( 'NONE',  ( 23.49999999999956657, -8.786575603324269439E-13, -6.000000000000000000 ) ) ;
#12367 = ADVANCED_FACE ( 'NONE', ( #2945 ), #14347, .F. ) ;
#12368 = FACE_OUTER_BOUND ( 'NONE', #9308, .T. ) ;
#12369 = CARTESIAN_POINT ( 'NONE',  ( -3.033343224707664376, 3.753672977998667726, -3.999999998634406140 ) ) ;
#12370 = SHAPE_DEFINITION_REPRESENTATION ( #15585, #4696 ) ;
#12371 = CARTESIAN_POINT ( 'NONE',  ( 4.799145180956616130, -0.5093500532425063732, -5.624999998634406140 ) ) ;
#12372 = CARTESIAN_POINT ( 'NONE',  ( -4.671041856245029322, -9.682850088987660890E-14, -0.2303389720127052009 ) ) ;
#12373 = ORIENTED_EDGE ( 'NONE', *, *, #13714, .F. ) ;
#12374 = CARTESIAN_POINT ( 'NONE',  ( 3.520694248372895352, -3.098194602941630738, -48.83371901636445500 ) ) ;
#12375 =( REPRESENTATION_RELATIONSHIP ('NONE','NONE', #4176, #279 ) REPRESENTATION_RELATIONSHIP_WITH_TRANSFORMATION ( #2683 )SHAPE_REPRESENTATION_RELATIONSHIP( ) );
#12376 = ADVANCED_FACE ( 'NONE', ( #10637 ), #1978, .T. ) ;
#12377 = ORIENTED_EDGE ( 'NONE', *, *, #2334, .T. ) ;
#12378 = DIRECTION ( 'NONE',  ( 0.5000000000000005551, 0.000000000000000000, -0.8660254037844382635 ) ) ;
#12379 = DIRECTION ( 'NONE',  ( 0.000000000000000000, 0.000000000000000000, 1.000000000000000000 ) ) ;
#12380 = ORIENTED_EDGE ( 'NONE', *, *, #5627, .T. ) ;
#12381 = CARTESIAN_POINT ( 'NONE',  ( 4.799145180956616130, -0.5093500532425063732, -1.624999998634406362 ) ) ;
#12382 = LINE ( 'NONE', #15145, #4000 ) ;
#12383 = CARTESIAN_POINT ( 'NONE',  ( 3.916244202832140253, -2.131511515620588160, -7.437499998634407916 ) ) ;
#12384 = CARTESIAN_POINT ( 'NONE',  ( 4.896370289181586344, -3.000000000000000000, 48.48076211353308906 ) ) ;
#12385 = UNCERTAINTY_MEASURE_WITH_UNIT (LENGTH_MEASURE( 1.000000000000000082E-05 ), #2512, 'distance_accuracy_value', 'NONE');
#12386 = DIRECTION ( 'NONE',  ( 0.000000000000000000, 0.000000000000000000, 1.000000000000000000 ) ) ;
#12387 = CARTESIAN_POINT ( 'NONE',  ( 2.390265326283148806, 4.391654775818395251, -2.749999997268815832 ) ) ;
#12388 = DIRECTION ( 'NONE',  ( -0.000000000000000000, -1.000000000000000000, -0.000000000000000000 ) ) ;
#12389 = CARTESIAN_POINT ( 'NONE',  ( -0.06609243105207880664, 4.488461494241831495, -0.3660093223227993686 ) ) ;
#12390 = CARTESIAN_POINT ( 'NONE',  ( -3.152801135295367985, -24.06250000136559564, 3.152801135295367096 ) ) ;
#12391 = ORIENTED_EDGE ( 'NONE', *, *, #5739, .T. ) ;
#12392 = CARTESIAN_POINT ( 'NONE',  ( 2.730187237215162345E-16, -22.18750000136559564, -4.458734124999999437 ) ) ;
#12393 = CARTESIAN_POINT ( 'NONE',  ( -0.5093500532425060401, -4.799145180956616130, -2.624999998634407028 ) ) ;
#12394 = CARTESIAN_POINT ( 'NONE',  ( -35.00000000000000000, 50.00000000000000000, -2.649999999999985700 ) ) ;
#12395 = EDGE_CURVE ( 'NONE', #12918, #9186, #444, .T. ) ;
#12396 = ORIENTED_EDGE ( 'NONE', *, *, #3559, .F. ) ;
#12397 = VERTEX_POINT ( 'NONE', #12796 ) ;
#12398 = EDGE_CURVE ( 'NONE', #3405, #513, #6598, .T. ) ;
#12399 = EDGE_LOOP ( 'NONE', ( #15802, #14800, #8439, #13228 ) ) ;
#12400 = CARTESIAN_POINT ( 'NONE',  ( -1.846868145590737420, -23.00000000136559564, 4.458734124999999437 ) ) ;
#12401 = CARTESIAN_POINT ( 'NONE',  ( -91.33974596215557540, -105.7735026918962689, 7.500000000000001776 ) ) ;
#12402 = CARTESIAN_POINT ( 'NONE',  ( 2.000000000000005329, -3.464101615137751722, 0.000000000000000000 ) ) ;
#12403 = CARTESIAN_POINT ( 'NONE',  ( -44.43375672974056556, -5.000000000000000000, 19.99999999999999645 ) ) ;
#12404 = CARTESIAN_POINT ( 'NONE',  ( -0.6249999999999978906, 8.299410119600878488, -7.298562697733107285 ) ) ;
#12405 = CARTESIAN_POINT ( 'NONE',  ( -44.99999999999999289, -35.00000000000000711, 7.500000000000001776 ) ) ;
#12406 = PRODUCT_DEFINITION_SHAPE ( 'NONE', 'NONE',  #15991 ) ;
#12407 = CARTESIAN_POINT ( 'NONE',  ( -5.381735091635034607, 0.5711823568785950878, -4.562500000000000000 ) ) ;
#12408 = CARTESIAN_POINT ( 'NONE',  ( 4.795541693661363958, 1.415196051561583790, -4.000000000000000000 ) ) ;
#12409 = CARTESIAN_POINT ( 'NONE',  ( -4.235886605889389145, -2.417314728048544303, -3.751161874094020909 ) ) ;
#12410 = CARTESIAN_POINT ( 'NONE',  ( 3.152801135295366208, -27.56250000136559564, 3.152801135295367985 ) ) ;
#12411 = CARTESIAN_POINT ( 'NONE',  ( -3.033343224707664376, 3.753672977998667726, -3.249999998634409692 ) ) ;
#12412 = VERTEX_POINT ( 'NONE', #6924 ) ;
#12413 = CARTESIAN_POINT ( 'NONE',  ( 0.000000000000000000, 0.000000000000000000, -4.000000000000000000 ) ) ;
#12414 = VERTEX_POINT ( 'NONE', #12718 ) ;
#12415 = ORIENTED_EDGE ( 'NONE', *, *, #13195, .F. ) ;
#12416 = ADVANCED_FACE ( 'NONE', ( #11668 ), #6839, .T. ) ;
#12417 = CARTESIAN_POINT ( 'NONE',  ( -4.000000000000000000, -2.512220745329312610, -3.469390707569719901 ) ) ;
#12418 = PRODUCT_DEFINITION ( 'UNKNOWN', '', #4050, #9974 ) ;
#12419 = CARTESIAN_POINT ( 'NONE',  ( -4.458734125000001214, -25.87500000136559919, 1.846868145590734089 ) ) ;
#12420 = LINE ( 'NONE', #5408, #8680 ) ;
#12421 = ORIENTED_EDGE ( 'NONE', *, *, #15462, .T. ) ;
#12422 = DIRECTION ( 'NONE',  ( 0.000000000000000000, 0.000000000000000000, 1.000000000000000000 ) ) ;
#12423 = VECTOR ( 'NONE', #10994, 1000.000000000000114 ) ;
#12424 =( BOUNDED_CURVE ( )  B_SPLINE_CURVE ( 2, ( #7062, #12942, #605, #9559, #6748, #6906, #14330, #915, #3257, #5839, #8204 ),
 .UNSPECIFIED., .F., .F. ) 
 B_SPLINE_CURVE_WITH_KNOTS ( ( 3, 2, 2, 2, 2, 3 ),
 ( 0.4045872658012772960, 0.4124999999999999778, 0.4249999999999999889, 0.4375000000000000000, 0.4500000000000000111, 0.4545872658012772849 ),
 .UNSPECIFIED. ) 
 CURVE ( )  GEOMETRIC_REPRESENTATION_ITEM ( )  RATIONAL_B_SPLINE_CURVE ( ( 0.9646335149384805963, 0.9518143178943438976, 1.000000000000000000, 0.9238795325112867385, 1.000000000000000000, 0.9238795325112867385, 1.000000000000000000, 0.9238795325112867385, 1.000000000000000000, 0.9720652146169430630, 0.9646335149384808183 ) ) 
 REPRESENTATION_ITEM ( '' )  );
#12425 = FACE_OUTER_BOUND ( 'NONE', #6460, .T. ) ;
#12426 = CARTESIAN_POINT ( 'NONE',  ( -1.261996585732579224, 4.276409079477648589, -3.062499998634407472 ) ) ;
#12427 = CARTESIAN_POINT ( 'NONE',  ( -67.50000000000000000, 37.00000000000000000, -7.070249711157346244E-13 ) ) ;
#12428 = CARTESIAN_POINT ( 'NONE',  ( -3.535533905932738641, -28.37500000000000000, 3.535533905932737309 ) ) ;
#12429 = FACE_OUTER_BOUND ( 'NONE', #15116, .T. ) ;
#12430 = CARTESIAN_POINT ( 'NONE',  ( 3.535533905932736864, -30.25000000273118417, 3.535533905932738641 ) ) ;
#12431 = DIRECTION ( 'NONE',  ( -0.000000000000000000, 1.000000000000000000, -0.000000000000000000 ) ) ;
#12432 = CARTESIAN_POINT ( 'NONE',  ( -1.846868145590734756, -29.12500000136559564, -4.458734124999999437 ) ) ;
#12433 = ADVANCED_FACE ( 'NONE', ( #3194 ), #11305, .F. ) ;
#12434 = DIRECTION ( 'NONE',  ( 0.000000000000000000, 0.000000000000000000, 1.000000000000000000 ) ) ;
#12435 = EDGE_LOOP ( 'NONE', ( #15763, #9034, #7094, #8750, #14427 ) ) ;
#12436 = EDGE_LOOP ( 'NONE', ( #5142, #13920, #15406, #6072, #5028, #15662, #7556 ) ) ;
#12437 = EDGE_CURVE ( 'NONE', #9361, #8804, #8445, .T. ) ;
#12438 = EDGE_CURVE ( 'NONE', #3972, #1651, #12025, .T. ) ;
#12439 = ORIENTED_EDGE ( 'NONE', *, *, #4912, .T. ) ;
#12440 = CARTESIAN_POINT ( 'NONE',  ( 7.703928834700302986, 4.447865386531934639, -7.917997657324739258 ) ) ;
#12441 = EDGE_LOOP ( 'NONE', ( #5442, #330, #14186, #1025 ) ) ;
#12442 = CARTESIAN_POINT ( 'NONE',  ( 0.000000000000000000, 0.000000000000000000, -25.03750572909317285 ) ) ;
#12443 = CARTESIAN_POINT ( 'NONE',  ( 3.152801135295367541, -31.56250000136559564, -3.152801135295367541 ) ) ;
#12444 = VECTOR ( 'NONE', #13087, 1000.000000000000000 ) ;
#12445 = CARTESIAN_POINT ( 'NONE',  ( 1.261996585732578113, -4.276409079477644148, -4.562499998634405252 ) ) ;
#12446 = CARTESIAN_POINT ( 'NONE',  ( -21.01110699893009581, 6.999999999999999112, 36.39230484541353405 ) ) ;
#12447 = CARTESIAN_POINT ( 'NONE',  ( 1.261996585732578113, -4.276409079477644148, -6.812499998634407028 ) ) ;
#12448 = FACE_OUTER_BOUND ( 'NONE', #10700, .T. ) ;
#12449 = FACE_OUTER_BOUND ( 'NONE', #1669, .T. ) ;
#12450 = ORIENTED_EDGE ( 'NONE', *, *, #12580, .T. ) ;
#12451 = DIRECTION ( 'NONE',  ( -0.000000000000000000, 1.000000000000000000, -0.000000000000000000 ) ) ;
#12452 = EDGE_CURVE ( 'NONE', #2123, #6666, #14888, .T. ) ;
#12453 = CIRCLE ( 'NONE', #6020, 2.500000000000000444 ) ;
#12454 = EDGE_LOOP ( 'NONE', ( #8989, #5836, #7953, #7433 ) ) ;
#12455 = CARTESIAN_POINT ( 'NONE',  ( 3.999999999999998224, 2.472263674411418588, -3.687027874309861897 ) ) ;
#12456 = DIRECTION ( 'NONE',  ( -0.000000000000000000, -1.000000000000000000, -0.000000000000000000 ) ) ;
#12457 = VERTEX_POINT ( 'NONE', #8591 ) ;
#12458 = CARTESIAN_POINT ( 'NONE',  ( -4.799145180956616130, 0.5093500532425063732, -5.124999998634406140 ) ) ;
#12459 = CARTESIAN_POINT ( 'NONE',  ( -3.916244202832140253, 2.131511515620587272, -7.937499998634408804 ) ) ;
#12460 = AXIS2_PLACEMENT_3D ( 'NONE', #5552, #7011, #8149 ) ;
#12461 = DIRECTION ( 'NONE',  ( 1.000000000000000000, 0.000000000000000000, 0.000000000000000000 ) ) ;
#12462 = DIRECTION ( 'NONE',  ( 0.000000000000000000, 0.000000000000000000, 1.000000000000000000 ) ) ;
#12463 = CARTESIAN_POINT ( 'NONE',  ( 3.401574460001763001, -4.209348295687703967, -3.062499997268815388 ) ) ;
#12464 = CARTESIAN_POINT ( 'NONE',  ( -4.391654775818395251, 2.390265326283148806, -8.499999997268814056 ) ) ;
#12465 = CARTESIAN_POINT ( 'NONE',  ( 5.000000000000000888, -28.06250000273118772, -2.071067811865475505 ) ) ;
#12467 = AXIS2_PLACEMENT_3D ( 'NONE', #1724, #536, #2047 ) ;
#12466 = CARTESIAN_POINT ( 'NONE',  ( -3.152801135295367985, -25.06250000136559564, 3.152801135295367096 ) ) ;
#12468 = ORIENTED_EDGE ( 'NONE', *, *, #10861, .F. ) ;
#12469 = LINE ( 'NONE', #1408, #9738 ) ;
#12470 = CARTESIAN_POINT ( 'NONE',  ( 3.753672977998667726, 3.033343224707664376, -7.249999998634409692 ) ) ;
#12471 = DIRECTION ( 'NONE',  ( 9.048317650695024227E-15, -0.000000000000000000, 1.000000000000000000 ) ) ;
#12472 = ORIENTED_EDGE ( 'NONE', *, *, #13615, .T. ) ;
#12473 = ORIENTED_EDGE ( 'NONE', *, *, #13958, .F. ) ;
#12474 = DIRECTION ( 'NONE',  ( 0.000000000000000000, 0.000000000000000000, 1.000000000000000000 ) ) ;
#12475 = ORIENTED_EDGE ( 'NONE', *, *, #13884, .T. ) ;
#12476 = CARTESIAN_POINT ( 'NONE',  ( -6.601567268551442602, 5.319966374295968414, -7.792327460285854102 ) ) ;
#12477 = CYLINDRICAL_SURFACE ( 'NONE', #14375, 5.000000000000000000 ) ;
#12478 = LINE ( 'NONE', #1510, #5549 ) ;
#12479 = EDGE_CURVE ( 'NONE', #10194, #3781, #10508, .T. ) ;
#12480 = CARTESIAN_POINT ( 'NONE',  ( 5.000000000000000888, -25.93750000000000711, -2.071067811865475505 ) ) ;
#12481 = CARTESIAN_POINT ( 'NONE',  ( -7.500000000000005329, 4.330127018922194537, -7.422398894150031623 ) ) ;
#12482 = AXIS2_PLACEMENT_3D ( 'NONE', #11778, #13151, #730 ) ;
#12483 = DIRECTION ( 'NONE',  ( 0.000000000000000000, 0.000000000000000000, -1.000000000000000000 ) ) ;
#12484 = CARTESIAN_POINT ( 'NONE',  ( -3.401574460001764777, 4.209348295687701302, -4.687500000000000888 ) ) ;
#12485 = DIRECTION ( 'NONE',  ( -0.000000000000000000, -1.000000000000000000, -0.000000000000000000 ) ) ;
#12486 = CARTESIAN_POINT ( 'NONE',  ( -14.99999999999998934, -1.734723475976807094E-15, 0.000000000000000000 ) ) ;
#12487 = CARTESIAN_POINT ( 'NONE',  ( 1.846868145590735200, -27.25000000136559564, -4.458734125000000326 ) ) ;
#12488 = CARTESIAN_POINT ( 'NONE',  ( -0.5093500532425060401, -4.799145180956616130, -1.874999998634406584 ) ) ;
#12489 = VERTEX_POINT ( 'NONE', #1375 ) ;
#12490 = LINE ( 'NONE', #14700, #11487 ) ;
#12491 = EDGE_LOOP ( 'NONE', ( #11643, #12858 ) ) ;
#12492 = VERTEX_POINT ( 'NONE', #7461 ) ;
#12493 = AXIS2_PLACEMENT_3D ( 'NONE', #917, #15951, #13254 ) ;
#12494 = CARTESIAN_POINT ( 'NONE',  ( 1.846868145590735200, -24.25000000136559564, -4.458734125000000326 ) ) ;
#12495 = DIRECTION ( 'NONE',  ( -0.000000000000000000, 0.000000000000000000, 1.000000000000000000 ) ) ;
#12496 = ORIENTED_EDGE ( 'NONE', *, *, #8002, .T. ) ;
#12497 = CARTESIAN_POINT ( 'NONE',  ( -4.000000000000000000, -1.942223658245633811, -0.3516579909967644246 ) ) ;
#12498 = PLANE ( 'NONE',  #7732 ) ;
#12499 = EDGE_CURVE ( 'NONE', #11995, #4136, #9948, .T. ) ;
#12500 = DIRECTION ( 'NONE',  ( 0.000000000000000000, 1.000000000000000000, 0.000000000000000000 ) ) ;
#12501 = CYLINDRICAL_SURFACE ( 'NONE', #12967, 5.000000000000000000 ) ;
#12502 = ADVANCED_FACE ( 'NONE', ( #10041 ), #14802, .F. ) ;
#12503 = CARTESIAN_POINT ( 'NONE',  ( -3.535533905932737309, -28.62500000000000000, -3.535533905932738197 ) ) ;
#12504 = CIRCLE ( 'NONE', #2189, 5.384454397937118664 ) ;
#12505 = PLANE ( 'NONE',  #2623 ) ;
#12506 = DIRECTION ( 'NONE',  ( 0.000000000000000000, 1.000000000000000000, 0.000000000000000000 ) ) ;
#12507 = CARTESIAN_POINT ( 'NONE',  ( 3.535533905932738197, -29.00000000273118772, -3.535533905932738197 ) ) ;
#12508 = STYLED_ITEM ( 'NONE', ( #3903 ), #14042 ) ;
#12509 = CARTESIAN_POINT ( 'NONE',  ( -44.99999999999999289, -35.00000000000000000, 7.500000000000001776 ) ) ;
#12510 = CARTESIAN_POINT ( 'NONE',  ( -4.458734125000000326, -28.87500000136559564, 1.846868145590734089 ) ) ;
#12511 = ORIENTED_EDGE ( 'NONE', *, *, #799, .T. ) ;
#12512 = ORIENTED_EDGE ( 'NONE', *, *, #12683, .F. ) ;
#12513 = VERTEX_POINT ( 'NONE', #4869 ) ;
#12514 = DIRECTION ( 'NONE',  ( 1.000000000000000000, 0.000000000000000000, 0.000000000000000000 ) ) ;
#12515 = VECTOR ( 'NONE', #12834, 1000.000000000000000 ) ;
#12516 = VERTEX_POINT ( 'NONE', #8303 ) ;
#12517 = CYLINDRICAL_SURFACE ( 'NONE', #15674, 5.000000000000000000 ) ;
#12518 = AXIS2_PLACEMENT_3D ( 'NONE', #14642, #3565, #8992 ) ;
#12519 = CIRCLE ( 'NONE', #11750, 2.649999999999985700 ) ;
#12520 = EDGE_CURVE ( 'NONE', #14811, #717, #8224, .T. ) ;
#12521 = DIRECTION ( 'NONE',  ( -0.000000000000000000, -1.000000000000000000, -0.000000000000000000 ) ) ;
#12522 = EDGE_CURVE ( 'NONE', #4598, #2810, #12541, .T. ) ;
#12523 = CARTESIAN_POINT ( 'NONE',  ( 2.730187237215162345E-16, -31.43750000136559564, -4.458734124999999437 ) ) ;
#12524 = DIRECTION ( 'NONE',  ( -3.061616997868333714E-17, 1.000000000000000000, 5.302876193624562924E-17 ) ) ;
#12525 = AXIS2_PLACEMENT_3D ( 'NONE', #11684, #12731, #5403 ) ;
#12526 = CARTESIAN_POINT ( 'NONE',  ( 3.033343224707661712, -3.753672977998669946, -3.749999998634409692 ) ) ;
#12527 = DIRECTION ( 'NONE',  ( 0.000000000000000000, 1.000000000000000000, 0.000000000000000000 ) ) ;
#12528 = CARTESIAN_POINT ( 'NONE',  ( -60.00000000000000000, -35.00000000000000000, -18.00000000000000000 ) ) ;
#12529 = ORIENTED_EDGE ( 'NONE', *, *, #15114, .F. ) ;
#12530 = VECTOR ( 'NONE', #15025, 1000.000000000000000 ) ;
#12531 = DIRECTION ( 'NONE',  ( 0.000000000000000000, -0.5000000000000011102, -0.8660254037844379305 ) ) ;
#12532 = ORIENTED_EDGE ( 'NONE', *, *, #1622, .F. ) ;
#12533 = CYLINDRICAL_SURFACE ( 'NONE', #10794, 2.649999999999992806 ) ;
#12534 = FACE_OUTER_BOUND ( 'NONE', #3660, .T. ) ;
#12535 = ORIENTED_EDGE ( 'NONE', *, *, #2334, .F. ) ;
#12536 = ITEM_DEFINED_TRANSFORMATION ( 'NONE', 'NONE', #14056,  #3223 ) ;
#12537 = CARTESIAN_POINT ( 'NONE',  ( -3.916244202832140253, 2.131511515620587272, -6.187499998634407028 ) ) ;
#12538 = VECTOR ( 'NONE', #14260, 1000.000000000000000 ) ;
#12539 = SURFACE_STYLE_FILL_AREA ( #7559 ) ;
#12540 = ADVANCED_FACE ( 'NONE', ( #2587 ), #7003, .F. ) ;
#12541 = CIRCLE ( 'NONE', #15926, 6.000000000000000888 ) ;
#12542 = EDGE_CURVE ( 'NONE', #10210, #8136, #5218, .T. ) ;
#12543 = DIRECTION ( 'NONE',  ( 0.5000000000000001110, 0.000000000000000000, -0.8660254037844384856 ) ) ;
#12544 = AXIS2_PLACEMENT_3D ( 'NONE', #12619, #9964, #9088 ) ;
#12545 = LINE ( 'NONE', #1567, #13086 ) ;
#12546 = PRODUCT_DEFINITION_CONTEXT ( 'detailed design', #8064, 'design' ) ;
#12547 = CARTESIAN_POINT ( 'NONE',  ( -2.500000000000000444, 3.061616997868383634E-16, -5.000000000000000888 ) ) ;
#12548 = CARTESIAN_POINT ( 'NONE',  ( 5.381735091635035495, -0.5711823568785978633, -2.937499997268817165 ) ) ;
#12549 = CARTESIAN_POINT ( 'NONE',  ( -45.00000000000000711, -2.452104961800526543E-15, 13.35786437626905077 ) ) ;
#12550 = CARTESIAN_POINT ( 'NONE',  ( -1.955611824408503674, 4.089455165765809141, -0.3290272460762475593 ) ) ;
#12551 = CARTESIAN_POINT ( 'NONE',  ( -3.152801135295367985, -23.06250000136559564, 3.152801135295367096 ) ) ;
#12552 = ORIENTED_EDGE ( 'NONE', *, *, #7626, .F. ) ;
#12553 = DIRECTION ( 'NONE',  ( 0.000000000000000000, 0.000000000000000000, 1.000000000000000000 ) ) ;
#12554 = CARTESIAN_POINT ( 'NONE',  ( -2.131511515620587272, -3.916244202832140253, -7.687499998634407916 ) ) ;
#12555 = CARTESIAN_POINT ( 'NONE',  ( -34.99999999999999289, -11.00000000000000178, -1.999999999999170441 ) ) ;
#12556 = EDGE_LOOP ( 'NONE', ( #5217, #6966, #11239, #6776, #7913 ) ) ;
#12557 = VERTEX_POINT ( 'NONE', #5018 ) ;
#12558 = CARTESIAN_POINT ( 'NONE',  ( -4.795541693661363958, -1.415196051561583790, 0.6250000027311839457 ) ) ;
#12559 = ORIENTED_EDGE ( 'NONE', *, *, #186, .T. ) ;
#12560 = DIRECTION ( 'NONE',  ( 0.000000000000000000, 1.000000000000000000, 0.000000000000000000 ) ) ;
#12561 = DIRECTION ( 'NONE',  ( -0.005931855436078210635, 0.9999824063907751803, 0.000000000000000000 ) ) ;
#12562 = CARTESIAN_POINT ( 'NONE',  ( 2.875844205642646756, -3.000000000000000000, 48.98110827882563711 ) ) ;
#12563 = CONICAL_SURFACE ( 'NONE', #12044, 2.500000000000000888, 0.9599310885968785900 ) ;
#12564 = EDGE_CURVE ( 'NONE', #13455, #8371, #5105, .T. ) ;
#12565 = DIRECTION ( 'NONE',  ( 0.000000000000000000, 0.000000000000000000, -1.000000000000000000 ) ) ;
#12566 = CARTESIAN_POINT ( 'NONE',  ( -6.484173630541807398, -4.916614646774628561, -7.642786413616653896 ) ) ;
#12567 = DIRECTION ( 'NONE',  ( 0.8660254037844387076, -0.000000000000000000, -0.4999999999999998890 ) ) ;
#12568 = AXIS2_PLACEMENT_3D ( 'NONE', #10840, #14719, #12190 ) ;
#12569 = CARTESIAN_POINT ( 'NONE',  ( 5.381735091635035495, -0.5711823568785978633, -7.062500000000005329 ) ) ;
#12570 = CARTESIAN_POINT ( 'NONE',  ( -1.415196051561583790, 4.795541693661363958, -2.750000000000002665 ) ) ;
#12571 = CARTESIAN_POINT ( 'NONE',  ( 0.000000000000000000, 0.000000000000000000, -4.974599999999998801 ) ) ;
#12572 = CARTESIAN_POINT ( 'NONE',  ( -4.458734125000001214, -23.87500000136559564, 1.846868145590734089 ) ) ;
#12573 = CARTESIAN_POINT ( 'NONE',  ( -0.5093500532425060401, -4.799145180956616130, -7.874999998634408804 ) ) ;
#12574 = EDGE_LOOP ( 'NONE', ( #13727, #7918, #8198, #13837 ) ) ;
#12575 = CIRCLE ( 'NONE', #5626, 2.649999999999992806 ) ;
#12576 = FACE_OUTER_BOUND ( 'NONE', #225, .T. ) ;
#12577 = ORIENTED_EDGE ( 'NONE', *, *, #294, .T. ) ;
#12578 = EDGE_LOOP ( 'NONE', ( #1753, #15250, #4580, #14217 ) ) ;
#12579 = CARTESIAN_POINT ( 'NONE',  ( 3.152801135295366208, -29.81250000136559208, 3.152801135295367985 ) ) ;
#12580 = EDGE_CURVE ( 'NONE', #13329, #11894, #5599, .T. ) ;
#12581 = CARTESIAN_POINT ( 'NONE',  ( 17.00000000000000000, 0.000000000000000000, 2.055000000000000160 ) ) ;
#12582 = EDGE_LOOP ( 'NONE', ( #15488, #12214, #9131, #5058 ) ) ;
#12583 = CIRCLE ( 'NONE', #15455, 32.00000000000000000 ) ;
#12584 = DIRECTION ( 'NONE',  ( 0.000000000000000000, 0.000000000000000000, -1.000000000000000000 ) ) ;
#12586 = AXIS2_PLACEMENT_3D ( 'NONE', #9220, #652, #5576 ) ;
#12585 = CARTESIAN_POINT ( 'NONE',  ( 0.000000000000000000, 40.00000000000000000, 0.000000000000000000 ) ) ;
#12587 = CARTESIAN_POINT ( 'NONE',  ( -3.916244202832140253, 2.131511515620587272, -0.9374999986344056957 ) ) ;
#12588 = DIRECTION ( 'NONE',  ( 0.000000000000000000, 0.000000000000000000, -1.000000000000000000 ) ) ;
#12589 = AXIS2_PLACEMENT_3D ( 'NONE', #2932, #5374, #6911 ) ;
#12590 = CARTESIAN_POINT ( 'NONE',  ( 5.000000000000000888, -29.93750000000000355, -2.071067811865475505 ) ) ;
#12591 = CARTESIAN_POINT ( 'NONE',  ( -4.999999999999999112, -5.773502691896264416, -7.063244554130005071 ) ) ;
#12592 = DIRECTION ( 'NONE',  ( -0.000000000000000000, -1.000000000000000000, -0.000000000000000000 ) ) ;
#12593 = CARTESIAN_POINT ( 'NONE',  ( -5.000000000000000888, -29.68750000273118772, -2.071067811865475949 ) ) ;
#12594 = CARTESIAN_POINT ( 'NONE',  ( 0.2500000000000002220, 0.000000000000000000, 0.000000000000000000 ) ) ;
#12595 = CARTESIAN_POINT ( 'NONE',  ( 4.458734124999999437, -31.37500000136559564, -1.846868145590734978 ) ) ;
#12596 = ORIENTED_EDGE ( 'NONE', *, *, #10086, .F. ) ;
#12597 = ORIENTED_EDGE ( 'NONE', *, *, #15217, .F. ) ;
#12599 = ORIENTED_EDGE ( 'NONE', *, *, #15815, .T. ) ;
#12598 = EDGE_CURVE ( 'NONE', #2379, #10415, #5773, .T. ) ;
#12600 = DIRECTION ( 'NONE',  ( 0.000000000000000000, 0.000000000000000000, -1.000000000000000000 ) ) ;
#12601 = VECTOR ( 'NONE', #2632, 1000.000000000000000 ) ;
#12602 = ADVANCED_FACE ( 'NONE', ( #15647 ), #6166, .T. ) ;
#12603 = CIRCLE ( 'NONE', #3335, 0.2000000000000000944 ) ;
#12604 = ORIENTED_EDGE ( 'NONE', *, *, #8343, .T. ) ;
#12605 = CARTESIAN_POINT ( 'NONE',  ( 7.894787914004607998, 1.231001383561881556E-13, -7.591390474663423760 ) ) ;
#12606 = VECTOR ( 'NONE', #14691, 1000.000000000000000 ) ;
#12607 = DIRECTION ( 'NONE',  ( 0.000000000000000000, 1.000000000000000000, 0.000000000000000000 ) ) ;
#12608 = CARTESIAN_POINT ( 'NONE',  ( -3.152801135295367096, -30.31250000136559564, -3.152801135295367541 ) ) ;
#12609 = CARTESIAN_POINT ( 'NONE',  ( -5.000000000000004441, -1.011557177027151181E-15, -6.420263044861759028 ) ) ;
#12610 = CARTESIAN_POINT ( 'NONE',  ( 3.753672977998667726, 3.033343224707664376, -7.499999998634409692 ) ) ;
#12611 = VECTOR ( 'NONE', #4220, 1000.000000000000000 ) ;
#12612 = FACE_OUTER_BOUND ( 'NONE', #6687, .T. ) ;
#12613 = ORIENTED_EDGE ( 'NONE', *, *, #1540, .T. ) ;
#12614 =( BOUNDED_CURVE ( )  B_SPLINE_CURVE ( 2, ( #10622, #7807, #15866, #12128, #2353, #3483, #1141, #7300, #836 ),
 .UNSPECIFIED., .F., .F. ) 
 B_SPLINE_CURVE_WITH_KNOTS ( ( 3, 2, 2, 2, 3 ),
 ( 0.3750000000000000000, 0.3875000000000000111, 0.4000000000000000222, 0.4125000000000000333, 0.4250000000000000444 ),
 .UNSPECIFIED. ) 
 CURVE ( )  GEOMETRIC_REPRESENTATION_ITEM ( )  RATIONAL_B_SPLINE_CURVE ( ( 1.000000000000000000, 0.9238795325112867385, 1.000000000000000000, 0.9238795325112867385, 1.000000000000000000, 0.9238795325112867385, 1.000000000000000000, 0.9238795325112864054, 1.000000000000000444 ) ) 
 REPRESENTATION_ITEM ( '' )  );
#12615 = CARTESIAN_POINT ( 'NONE',  ( 0.000000000000000000, -20.00000000000000000, 5.000000000000000000 ) ) ;
#12616 = FILL_AREA_STYLE ('',( #5198 ) ) ;
#12617 = ORIENTED_EDGE ( 'NONE', *, *, #14803, .F. ) ;
#12618 = LINE ( 'NONE', #1560, #12611 ) ;
#12619 = CARTESIAN_POINT ( 'NONE',  ( 0.000000000000000000, 0.000000000000000000, 0.000000000000000000 ) ) ;
#12620 = EDGE_CURVE ( 'NONE', #14899, #9639, #1713, .T. ) ;
#12621 = VERTEX_POINT ( 'NONE', #7296 ) ;
#12622 = CONTEXT_DEPENDENT_SHAPE_REPRESENTATION ( #537, #15288 ) ;
#12623 = CARTESIAN_POINT ( 'NONE',  ( 1.261996585732578113, -4.276409079477644148, -6.812499998634407028 ) ) ;
#12624 = CARTESIAN_POINT ( 'NONE',  ( 4.209348295687701302, 3.401574460001766109, -4.812499997268817609 ) ) ;
#12625 = DIRECTION ( 'NONE',  ( 0.000000000000000000, 0.000000000000000000, -1.000000000000000000 ) ) ;
#12626 = CYLINDRICAL_SURFACE ( 'NONE', #9731, 5.000000000000000000 ) ;
#12627 = CARTESIAN_POINT ( 'NONE',  ( -4.000000000000000000, 2.309401076758498483, -3.433295621305379353 ) ) ;
#12628 = CARTESIAN_POINT ( 'NONE',  ( 1.415196051561583790, -4.795541693661363958, -4.124999997268816720 ) ) ;
#12629 = CARTESIAN_POINT ( 'NONE',  ( -39.99999999999999289, -13.00000000000000178, 2.500000000001739497 ) ) ;
#12630 = CARTESIAN_POINT ( 'NONE',  ( 2.071067811865482611, -27.93750000273118772, -4.999999999999992895 ) ) ;
#12631 = CARTESIAN_POINT ( 'NONE',  ( 4.458734124999997661, -22.75000000136559919, 1.846868145590737864 ) ) ;
#12632 = ORIENTED_EDGE ( 'NONE', *, *, #14135, .T. ) ;
#12633 = CARTESIAN_POINT ( 'NONE',  ( 0.000000000000000000, 20.00000000000000000, 0.000000000000000000 ) ) ;
#12634 = CARTESIAN_POINT ( 'NONE',  ( -1.261996585732579224, 4.276409079477648589, -8.062499998634407916 ) ) ;
#12635 = DIRECTION ( 'NONE',  ( -0.000000000000000000, -0.000000000000000000, 1.000000000000000000 ) ) ;
#12636 = ADVANCED_FACE ( 'NONE', ( #2419 ), #12199, .T. ) ;
#12637 = VERTEX_POINT ( 'NONE', #7372 ) ;
#12638 = ORIENTED_EDGE ( 'NONE', *, *, #10158, .T. ) ;
#12639 = ADVANCED_FACE ( 'NONE', ( #27, #11634 ), #8913, .T. ) ;
#12640 = ADVANCED_FACE ( 'NONE', ( #2993 ), #2910, .F. ) ;
#12641 = EDGE_CURVE ( 'NONE', #11577, #9381, #8610, .T. ) ;
#12642 = EDGE_LOOP ( 'NONE', ( #8787, #8298, #12661 ) ) ;
#12643 = CARTESIAN_POINT ( 'NONE',  ( 1.415196051561583790, -4.795541693661363958, -0.2500000000000036637 ) ) ;
#12644 = DIRECTION ( 'NONE',  ( -0.000000000000000000, 1.471414886128461471E-15, 1.000000000000000000 ) ) ;
#12645 = LINE ( 'NONE', #6521, #11726 ) ;
#12646 = CARTESIAN_POINT ( 'NONE',  ( 5.000000000000000000, -26.06250000000000355, 2.071067811865478614 ) ) ;
#12647 = CARTESIAN_POINT ( 'NONE',  ( -3.750000000000011102, 6.495190528383311346, -6.991905250253764414 ) ) ;
#12648 = LINE ( 'NONE', #2551, #5904 ) ;
#12649 = CARTESIAN_POINT ( 'NONE',  ( 1.415196051561583790, -4.795541693661363958, -4.250000000000000000 ) ) ;
#12650 = DIRECTION ( 'NONE',  ( 0.000000000000000000, 0.000000000000000000, -1.000000000000000000 ) ) ;
#12651 = CARTESIAN_POINT ( 'NONE',  ( 0.1756481739660539498, -4.720212674038995360, -3.469390959564070620 ) ) ;
#12652 = CARTESIAN_POINT ( 'NONE',  ( 4.458734124999999437, -21.50000000136559208, 1.846868145590737864 ) ) ;
#12653 = CARTESIAN_POINT ( 'NONE',  ( -3.033343224707664376, 3.753672977998667726, -6.249999998634408804 ) ) ;
#12654 = ORIENTED_EDGE ( 'NONE', *, *, #14245, .T. ) ;
#12655 = CARTESIAN_POINT ( 'NONE',  ( 2.500000000000000000, 0.000000000000000000, 0.000000000000000000 ) ) ;
#12656 = ORIENTED_EDGE ( 'NONE', *, *, #14005, .F. ) ;
#12657 = VERTEX_POINT ( 'NONE', #5188 ) ;
#12658 = ADVANCED_FACE ( 'NONE', ( #6407 ), #10288, .T. ) ;
#12659 = CARTESIAN_POINT ( 'NONE',  ( 4.458734124999999437, -22.43750000136559564, 0.000000000000000000 ) ) ;
#12660 = CARTESIAN_POINT ( 'NONE',  ( -91.33974596215560382, -110.0591436588189396, -7.500000000000001776 ) ) ;
#12661 = ORIENTED_EDGE ( 'NONE', *, *, #6147, .F. ) ;
#12662 = CARTESIAN_POINT ( 'NONE',  ( -5.000000000000000888, -28.43750000000000355, 2.071067811865474617 ) ) ;
#12663 = LINE ( 'NONE', #332, #10310 ) ;
#12664 = CARTESIAN_POINT ( 'NONE',  ( 0.000000000000000000, -13.00000000000000178, 1.500000000000000000 ) ) ;
#12665 = DIRECTION ( 'NONE',  ( 0.000000000000000000, 0.000000000000000000, 1.000000000000000000 ) ) ;
#12666 = CARTESIAN_POINT ( 'NONE',  ( -2.071067811865478170, -29.31250000000000000, 5.000000000000000000 ) ) ;
#12667 = CARTESIAN_POINT ( 'NONE',  ( -44.01347164682042035, -3.060691311048526764, -21.49473191792460014 ) ) ;
#12668 = CARTESIAN_POINT ( 'NONE',  ( 6.000000000000000000, -13.00000000000000178, 0.000000000000000000 ) ) ;
#12669 = CARTESIAN_POINT ( 'NONE',  ( 5.000000000000000888, -26.06250000273118417, -2.071067811865475505 ) ) ;
#12670 = CARTESIAN_POINT ( 'NONE',  ( 4.458734124999999437, -26.43750000136559564, 0.000000000000000000 ) ) ;
#12671 = DIRECTION ( 'NONE',  ( -0.000000000000000000, 1.000000000000000000, -0.000000000000000000 ) ) ;
#12672 = ORIENTED_EDGE ( 'NONE', *, *, #11368, .T. ) ;
#12673 = VERTEX_POINT ( 'NONE', #5350 ) ;
#12674 = PRODUCT_DEFINITION_SHAPE ( 'NONE', 'NONE',  #15979 ) ;
#12675 = ORIENTED_EDGE ( 'NONE', *, *, #10856, .F. ) ;
#12676 = CARTESIAN_POINT ( 'NONE',  ( -124.9999999999999858, -115.2072594216369907, -7.500000000000000000 ) ) ;
#12677 = VECTOR ( 'NONE', #5946, 1000.000000000000000 ) ;
#12678 = VERTEX_POINT ( 'NONE', #514 ) ;
#12679 = LINE ( 'NONE', #11560, #5086 ) ;
#12680 = DIRECTION ( 'NONE',  ( 0.000000000000000000, 0.000000000000000000, -1.000000000000000000 ) ) ;
#12681 = CARTESIAN_POINT ( 'NONE',  ( -7.894787914004613327, -1.222495057920810896E-13, -7.591390474663425536 ) ) ;
#12682 = CARTESIAN_POINT ( 'NONE',  ( 19.99999999999956657, -8.786575603324269439E-13, -6.000000000000000000 ) ) ;
#12683 = EDGE_CURVE ( 'NONE', #7238, #10747, #12679, .T. ) ;
#12684 = EDGE_CURVE ( 'NONE', #8282, #10516, #15216, .T. ) ;
#12685 = ITEM_DEFINED_TRANSFORMATION ( 'NONE', 'NONE', #12493,  #3223 ) ;
#12686 = CARTESIAN_POINT ( 'NONE',  ( 5.000000000000000000, -5.773502691896266192, -7.063244554130005071 ) ) ;
#12687 = CARTESIAN_POINT ( 'NONE',  ( -17.99999999999979394, -9.000000000000001776, 1.499999999999999112 ) ) ;
#12688 = EDGE_LOOP ( 'NONE', ( #9166, #1647, #14258, #12955 ) ) ;
#12689 =( LENGTH_UNIT ( ) NAMED_UNIT ( * ) SI_UNIT ( .MILLI., .METRE. ) );
#12690 = VERTEX_POINT ( 'NONE', #7946 ) ;
#12691 = LINE ( 'NONE', #1634, #14692 ) ;
#12692 = CARTESIAN_POINT ( 'NONE',  ( 0.000000000000000000, -11.00000000000000178, 0.000000000000000000 ) ) ;
#12693 = ORIENTED_EDGE ( 'NONE', *, *, #7074, .T. ) ;
#12694 = CARTESIAN_POINT ( 'NONE',  ( -4.276409079477644148, -1.261996585732578335, -5.062499998634406140 ) ) ;
#12695 = VECTOR ( 'NONE', #2837, 1000.000000000000000 ) ;
#12696 = CARTESIAN_POINT ( 'NONE',  ( -1.415196051561583790, 4.795541693661363958, -4.624999997268817609 ) ) ;
#12697 = CIRCLE ( 'NONE', #6783, 4.999999999999997335 ) ;
#12698 = CARTESIAN_POINT ( 'NONE',  ( -0.5711823568785977523, -5.381735091635034607, -5.187499997268819385 ) ) ;
#12699 = EDGE_CURVE ( 'NONE', #4101, #4042, #6560, .T. ) ;
#12700 = LINE ( 'NONE', #9094, #4569 ) ;
#12701 = EDGE_CURVE ( 'NONE', #4620, #12414, #1462, .T. ) ;
#12702 = UNCERTAINTY_MEASURE_WITH_UNIT (LENGTH_MEASURE( 1.000000000000000082E-05 ), #6481, 'distance_accuracy_value', 'NONE');
#12703 = CARTESIAN_POINT ( 'NONE',  ( -0.5711823568785978633, -5.381735091635035495, -4.187499997268818497 ) ) ;
#12704 = CARTESIAN_POINT ( 'NONE',  ( -2.071067811865489272, -23.68749999999999645, -4.999999999999985789 ) ) ;
#12705 = CARTESIAN_POINT ( 'NONE',  ( 17.00000000000000000, 0.000000000000000000, 2.055000000000000160 ) ) ;
#12706 = CARTESIAN_POINT ( 'NONE',  ( -91.33974596215558961, -105.7735026918962262, -7.500000000000000000 ) ) ;
#12707 = ORIENTED_EDGE ( 'NONE', *, *, #14247, .T. ) ;
#12708 = CARTESIAN_POINT ( 'NONE',  ( -21.01110699893041911, 0.000000000000000000, -36.39230484541334221 ) ) ;
#12709 = CARTESIAN_POINT ( 'NONE',  ( -4.799145180956616130, 0.5093500532425063732, -7.874999998634408804 ) ) ;
#12710 = AXIS2_PLACEMENT_3D ( 'NONE', #13191, #697, #5623 ) ;
#12711 = CARTESIAN_POINT ( 'NONE',  ( -6.765421556309547668E-13, 37.00000000000000000, 64.84999999999932641 ) ) ;
#12712 = ORIENTED_EDGE ( 'NONE', *, *, #8122, .F. ) ;
#12713 = VECTOR ( 'NONE', #6628, 1000.000000000000000 ) ;
#12714 = CARTESIAN_POINT ( 'NONE',  ( -4.197477534772231955, 0.8522413273724368521, -3.505042416683225692 ) ) ;
#12715 = ORIENTED_EDGE ( 'NONE', *, *, #10019, .F. ) ;
#12716 = ORIENTED_EDGE ( 'NONE', *, *, #2548, .F. ) ;
#12717 = CARTESIAN_POINT ( 'NONE',  ( 67.49999999999931788, 50.00000000000000000, 2.081668171172168513E-14 ) ) ;
#12718 = CARTESIAN_POINT ( 'NONE',  ( -9.184850993605147944E-16, -25.25000000000000000, 5.000000000000000000 ) ) ;
#12719 = CARTESIAN_POINT ( 'NONE',  ( 2.500000000000000000, 1.178949249685213863, -2.042000000000001148 ) ) ;
#12720 = ADVANCED_FACE ( 'NONE', ( #7619 ), #8994, .T. ) ;
#12721 = CARTESIAN_POINT ( 'NONE',  ( -43.99999999999978684, -9.000000000000001776, 1.499999999999998668 ) ) ;
#12722 = CARTESIAN_POINT ( 'NONE',  ( 2.602085213965210642E-15, 8.660254037844392627, -7.422398894150035176 ) ) ;
#12723 = EDGE_CURVE ( 'NONE', #865, #9569, #14122, .T. ) ;
#12724 = FACE_OUTER_BOUND ( 'NONE', #5296, .T. ) ;
#12725 = CARTESIAN_POINT ( 'NONE',  ( 3.401574460001763001, -4.209348295687703967, -4.187500000000000888 ) ) ;
#12726 = CARTESIAN_POINT ( 'NONE',  ( -31.74999999999995737, 0.000000000000000000, 2.500000000000000888 ) ) ;
#12727 = CARTESIAN_POINT ( 'NONE',  ( 0.000000000000000000, -1.178949249685213863, 2.042000000000002924 ) ) ;
#12728 = CARTESIAN_POINT ( 'NONE',  ( 1.846868145590735200, -23.25000000136559208, -4.458734125000000326 ) ) ;
#12729 = CARTESIAN_POINT ( 'NONE',  ( 4.276409079477644148, 1.261996585732577891, -6.562499998634407028 ) ) ;
#12730 = ORIENTED_EDGE ( 'NONE', *, *, #3832, .F. ) ;
#12731 = DIRECTION ( 'NONE',  ( -1.239088197126290570E-16, 0.000000000000000000, -1.000000000000000000 ) ) ;
#12732 = ORIENTED_EDGE ( 'NONE', *, *, #2709, .T. ) ;
#12733 = ORIENTED_EDGE ( 'NONE', *, *, #12143, .T. ) ;
#12734 = CARTESIAN_POINT ( 'NONE',  ( -4.458734124999999437, -30.18750000136559564, -5.460374474430324690E-16 ) ) ;
#12735 = LINE ( 'NONE', #12581, #12530 ) ;
#12736 = EDGE_LOOP ( 'NONE', ( #15350, #8552 ) ) ;
#12737 = CARTESIAN_POINT ( 'NONE',  ( 4.236525694536557474, -2.416953475386482530, -3.751298745799839462 ) ) ;
#12738 = VECTOR ( 'NONE', #6788, 1000.000000000000000 ) ;
#12739 = CARTESIAN_POINT ( 'NONE',  ( 7.500000000000000000, -3.157198044629319522, -7.642795354507490480 ) ) ;
#12740 = EDGE_CURVE ( 'NONE', #5460, #8492, #9990, .T. ) ;
#12741 = FACE_OUTER_BOUND ( 'NONE', #9848, .T. ) ;
#12742 = CARTESIAN_POINT ( 'NONE',  ( 0.000000000000000000, -20.00000000000000000, 5.000000000000000000 ) ) ;
#12743 = ADVANCED_FACE ( 'NONE', ( #4127 ), #6649, .F. ) ;
#12744 = CARTESIAN_POINT ( 'NONE',  ( -5.000000000000000000, -29.50000000000000355, -6.123233995736766282E-16 ) ) ;
#12745 = CARTESIAN_POINT ( 'NONE',  ( 2.131511515620586383, 3.916244202832140253, -5.187499998634406140 ) ) ;
#12746 = CARTESIAN_POINT ( 'NONE',  ( 7.500000000000000888, 4.330127018922199866, -1.000000000000000888 ) ) ;
#12747 = CARTESIAN_POINT ( 'NONE',  ( 7.500000000000003553, -4.330127018922199866, -9.999999999999998224 ) ) ;
#12748 = CARTESIAN_POINT ( 'NONE',  ( 3.535533905932738197, -26.00000000273118417, -3.535533905932738197 ) ) ;
#12749 = CARTESIAN_POINT ( 'NONE',  ( -2.390265326283148806, -4.391654775818394363, -3.375000000000003109 ) ) ;
#12750 = CARTESIAN_POINT ( 'NONE',  ( -1.846868145590734756, -25.12500000136559564, -4.458734124999999437 ) ) ;
#12751 = CARTESIAN_POINT ( 'NONE',  ( 2.558993250141106568, -7.638875775591494666, -7.593821156097298797 ) ) ;
#12752 = VERTEX_POINT ( 'NONE', #8831 ) ;
#12753 = VERTEX_POINT ( 'NONE', #11398 ) ;
#12754 = AXIS2_PLACEMENT_3D ( 'NONE', #10569, #4245, #5466 ) ;
#12755 = ORIENTED_EDGE ( 'NONE', *, *, #11833, .T. ) ;
#12756 = CARTESIAN_POINT ( 'NONE',  ( -44.43375672974056556, -5.000000000000000000, 19.99999999999999645 ) ) ;
#12757 = ORIENTED_EDGE ( 'NONE', *, *, #3164, .F. ) ;
#12758 = CARTESIAN_POINT ( 'NONE',  ( 7.914984360234579519, -3.818534719232097530, -7.907701344400641652 ) ) ;
#12759 = VECTOR ( 'NONE', #15487, 1000.000000000000000 ) ;
#12760 = CARTESIAN_POINT ( 'NONE',  ( 2.390265326283148806, 4.391654775818395251, -1.749999997268814722 ) ) ;
#12761 = ADVANCED_FACE ( 'NONE', ( #15295 ), #12517, .T. ) ;
#12762 = CARTESIAN_POINT ( 'NONE',  ( 4.458734124999999437, -29.68750000136559208, 0.000000000000000000 ) ) ;
#12763 = CARTESIAN_POINT ( 'NONE',  ( 4.769696007084728073, -20.00000000000000000, -1.500000000000000000 ) ) ;
#12764 = ITEM_DEFINED_TRANSFORMATION ( 'NONE', 'NONE', #14568,  #3223 ) ;
#12765 = CARTESIAN_POINT ( 'NONE',  ( 3.753672977998667726, 3.033343224707664376, -8.499999998634411469 ) ) ;
#12766 = CARTESIAN_POINT ( 'NONE',  ( -31.74999999999995737, 5.204748896376250699E-16, -4.250000000000000000 ) ) ;
#12767 = ORIENTED_EDGE ( 'NONE', *, *, #4185, .F. ) ;
#12768 = SURFACE_STYLE_FILL_AREA ( #9008 ) ;
#12769 = VERTEX_POINT ( 'NONE', #350 ) ;
#12770 = LINE ( 'NONE', #1799, #2552 ) ;
#12771 = CARTESIAN_POINT ( 'NONE',  ( 2.730187237215162345E-16, -30.18750000136559564, -4.458734124999999437 ) ) ;
#12772 = CIRCLE ( 'NONE', #13540, 3.499999999999999556 ) ;
#12773 = ORIENTED_EDGE ( 'NONE', *, *, #4639, .T. ) ;
#12774 = APPLICATION_CONTEXT ( 'automotive_design' ) ;
#12775 = EDGE_CURVE ( 'NONE', #15821, #2497, #194, .T. ) ;
#12776 = CARTESIAN_POINT ( 'NONE',  ( 35.00000000000000000, 37.00000000000000000, -5.999999999999991118 ) ) ;
#12777 = CIRCLE ( 'NONE', #6885, 2.649999999999985700 ) ;
#12778 = DIRECTION ( 'NONE',  ( 1.734723475976810299E-16, -1.000000000000000000, 0.000000000000000000 ) ) ;
#12779 = CARTESIAN_POINT ( 'NONE',  ( 2.000000000000005329, -3.464101615137751722, 0.000000000000000000 ) ) ;
#12780 = AXIS2_PLACEMENT_3D ( 'NONE', #12660, #1529, #15100 ) ;
#12781 = CARTESIAN_POINT ( 'NONE',  ( 3.401574460001763001, -4.209348295687703967, -8.062499997268812280 ) ) ;
#12782 = FACE_OUTER_BOUND ( 'NONE', #6138, .T. ) ;
#12783 = CARTESIAN_POINT ( 'NONE',  ( 1.846868145590735200, -22.50000000136559564, -4.458734124999999437 ) ) ;
#12784 = ORIENTED_EDGE ( 'NONE', *, *, #14213, .T. ) ;
#12785 = DIRECTION ( 'NONE',  ( 0.000000000000000000, 0.000000000000000000, -1.000000000000000000 ) ) ;
#12786 = CARTESIAN_POINT ( 'NONE',  ( 7.500000000000001776, -2.886751345948134873, -7.198902722707430257 ) ) ;
#12787 = DIRECTION ( 'NONE',  ( 0.000000000000000000, 1.000000000000000000, 0.000000000000000000 ) ) ;
#12788 = EDGE_LOOP ( 'NONE', ( #7659, #5559, #1795, #1310 ) ) ;
#12789 = LINE ( 'NONE', #1276, #6673 ) ;
#12790 = AXIS2_PLACEMENT_3D ( 'NONE', #1471, #11332, #15133 ) ;
#12791 = ORIENTED_EDGE ( 'NONE', *, *, #100, .F. ) ;
#12792 = VECTOR ( 'NONE', #6441, 1000.000000000000000 ) ;
#12793 = ORIENTED_EDGE ( 'NONE', *, *, #446, .F. ) ;
#12794 = CYLINDRICAL_SURFACE ( 'NONE', #13069, 2.649999999999992806 ) ;
#12795 = EDGE_CURVE ( 'NONE', #15708, #1389, #6646, .T. ) ;
#12796 = CARTESIAN_POINT ( 'NONE',  ( -17.99999999999979394, -9.000000000000001776, 3.499999999999998668 ) ) ;
#12797 = EDGE_CURVE ( 'NONE', #12657, #2074, #6884, .T. ) ;
#12798 = AXIS2_PLACEMENT_3D ( 'NONE', #548, #10476, #15494 ) ;
#12799 = CARTESIAN_POINT ( 'NONE',  ( 4.000000000000000000, -1.084202172485504434E-14, -3.142992957459231906 ) ) ;
#12800 = AXIS2_PLACEMENT_3D ( 'NONE', #13749, #11490, #12379 ) ;
#12801 = CARTESIAN_POINT ( 'NONE',  ( -35.00000000000000000, 50.00000000000000000, 2.649999999999992806 ) ) ;
#12803 = CARTESIAN_POINT ( 'NONE',  ( 4.000000000000000000, 2.309401076758497151, -5.000000000000000000 ) ) ;
#12802 = AXIS2_PLACEMENT_3D ( 'NONE', #5468, #7987, #5392 ) ;
#12804 = DIRECTION ( 'NONE',  ( 0.000000000000000000, 0.000000000000000000, -1.000000000000000000 ) ) ;
#12805 = CARTESIAN_POINT ( 'NONE',  ( 4.209348295687701302, 3.401574460001765665, -7.937500000000003553 ) ) ;
#12806 = CARTESIAN_POINT ( 'NONE',  ( -21.01110699893041556, 0.000000000000000000, -33.74230484541335073 ) ) ;
#12807 = DIRECTION ( 'NONE',  ( 0.000000000000000000, 0.000000000000000000, -1.000000000000000000 ) ) ;
#12808 = CARTESIAN_POINT ( 'NONE',  ( 4.458734125000000326, -23.37500000136559564, -1.846868145590734978 ) ) ;
#12809 = AXIS2_PLACEMENT_3D ( 'NONE', #13569, #13415, #13251 ) ;
#12810 = CARTESIAN_POINT ( 'NONE',  ( 0.5093500532425063732, 4.799145180956616130, -6.374999998634407028 ) ) ;
#12811 = ORIENTED_EDGE ( 'NONE', *, *, #2998, .F. ) ;
#12812 = DIRECTION ( 'NONE',  ( 0.000000000000000000, 0.000000000000000000, 1.000000000000000000 ) ) ;
#12813 = ORIENTED_EDGE ( 'NONE', *, *, #9578, .T. ) ;
#12814 = ORIENTED_EDGE ( 'NONE', *, *, #2079, .T. ) ;
#12815 = ORIENTED_EDGE ( 'NONE', *, *, #13324, .T. ) ;
#12816 = CARTESIAN_POINT ( 'NONE',  ( -1.846868145590737420, -31.00000000136559564, 4.458734124999999437 ) ) ;
#12817 = ADVANCED_FACE ( 'NONE', ( #14157 ), #3015, .T. ) ;
#12818 = CYLINDRICAL_SURFACE ( 'NONE', #8950, 2.649999999999985700 ) ;
#12819 = AXIS2_PLACEMENT_3D ( 'NONE', #3017, #7963, #12868 ) ;
#12820 = EDGE_CURVE ( 'NONE', #12673, #8490, #10766, .T. ) ;
#12821 = ORIENTED_EDGE ( 'NONE', *, *, #7708, .T. ) ;
#12822 = CARTESIAN_POINT ( 'NONE',  ( -19.99999999999956657, -9.000000000000001776, 2.500000000000877520 ) ) ;
#12823 = CARTESIAN_POINT ( 'NONE',  ( 7.894958282449826115, -1.603399432392641266, -7.593838100136975022 ) ) ;
#12824 = CARTESIAN_POINT ( 'NONE',  ( -3.753672977998669502, -3.033343224707661712, -3.749999998634410137 ) ) ;
#12825 = CARTESIAN_POINT ( 'NONE',  ( 21.99999999999956657, -8.786575603324269439E-13, -4.500000000000000000 ) ) ;
#12826 = CARTESIAN_POINT ( 'NONE',  ( -9.184850993605147944E-16, -25.25000000000000000, 5.000000000000000000 ) ) ;
#12827 = CARTESIAN_POINT ( 'NONE',  ( -4.799145180956616130, 0.5093500532425063732, -4.874999998634405252 ) ) ;
#12828 = CARTESIAN_POINT ( 'NONE',  ( 1.411581201560190495E-15, 4.862606272033091592, -3.745885042887436622 ) ) ;
#12829 = AXIS2_PLACEMENT_3D ( 'NONE', #1364, #9065, #412 ) ;
#12830 = DIRECTION ( 'NONE',  ( 0.000000000000000000, 1.000000000000000000, 0.000000000000000000 ) ) ;
#12831 = CARTESIAN_POINT ( 'NONE',  ( -2.071067811865475061, -25.81250000273118417, -5.000000000000000888 ) ) ;
#12832 = DIRECTION ( 'NONE',  ( 0.000000000000000000, -1.000000000000000000, 0.000000000000000000 ) ) ;
#12833 = CARTESIAN_POINT ( 'NONE',  ( -3.152801135295367985, -24.81250000136559564, 3.152801135295367096 ) ) ;
#12834 = DIRECTION ( 'NONE',  ( 0.000000000000000000, -1.000000000000000000, 0.000000000000000000 ) ) ;
#12835 = VERTEX_POINT ( 'NONE', #2175 ) ;
#12836 = VERTEX_POINT ( 'NONE', #3158 ) ;
#12837 = CARTESIAN_POINT ( 'NONE',  ( 3.061616997868383141E-16, -28.87500000273118772, -5.000000000000000000 ) ) ;
#12839 = EDGE_CURVE ( 'NONE', #2808, #8889, #13007, .T. ) ;
#12838 = ORIENTED_EDGE ( 'NONE', *, *, #2831, .T. ) ;
#12840 = CARTESIAN_POINT ( 'NONE',  ( 5.000000000000000888, -29.06250000273118772, -2.071067811865475505 ) ) ;
#12841 = EDGE_CURVE ( 'NONE', #13728, #14177, #11396, .T. ) ;
#12842 = EDGE_CURVE ( 'NONE', #12621, #1848, #9542, .T. ) ;
#12843 = ORIENTED_EDGE ( 'NONE', *, *, #11418, .F. ) ;
#12844 = DIRECTION ( 'NONE',  ( 0.000000000000000000, 0.000000000000000000, -1.000000000000000000 ) ) ;
#12845 = VECTOR ( 'NONE', #9758, 1000.000000000000000 ) ;
#12846 = PRODUCT_DEFINITION_SHAPE ( 'NONE', 'NONE',  #6223 ) ;
#12847 = LINE ( 'NONE', #13002, #10914 ) ;
#12848 = CARTESIAN_POINT ( 'NONE',  ( 3.152801135295366208, -28.81250000136559564, 3.152801135295367985 ) ) ;
#12849 = VECTOR ( 'NONE', #2894, 1000.000000000000000 ) ;
#12850 = CARTESIAN_POINT ( 'NONE',  ( 5.000000000000004441, -2.247904837838113790E-16, -6.920263044861760804 ) ) ;
#12851 = PRODUCT_CONTEXT ( 'NONE', #2873, 'mechanical' ) ;
#12852 =( BOUNDED_SURFACE ( )  B_SPLINE_SURFACE ( 3, 2, ( 
 ( #14151, #1783, #3080 ),
 ( #3155, #8100, #3625 ),
 ( #3457, #1041, #5976 ),
 ( #2167, #969, #8337 ),
 ( #6053, #1113, #9538 ),
 ( #3, #14539, #2248 ),
 ( #4919, #3699, #11066 ),
 ( #10898, #8644, #9845 ) ),
 .UNSPECIFIED., .F., .F., .T. ) 
 B_SPLINE_SURFACE_WITH_KNOTS ( ( 4, 2, 2, 4 ),
 ( 3, 3 ),
 ( 0.03851319102641418551, 0.04314724750133522302, 0.04546427573879573830, 0.04778130397625625359 ),
 ( 0.000000000000000000, 1.000000000000000000 ),
 .UNSPECIFIED. ) 
 GEOMETRIC_REPRESENTATION_ITEM ( )  RATIONAL_B_SPLINE_SURFACE ( (
 ( 1.000000000000000000, 0.8047781573724569482, 1.000000000000000000),
 ( 1.000000000000000000, 0.8123768202407034567, 1.000000000000000000),
 ( 1.000000000000000000, 0.8190667609308863728, 1.000000000000000000),
 ( 1.000000000000000000, 0.8191933927156080930, 1.000000000000000000),
 ( 1.000000000000000000, 0.8176088169850975751, 1.000000000000000000),
 ( 1.000000000000000000, 0.8122958474541809304, 1.000000000000000000),
 ( 1.000000000000000000, 0.8086309703845759866, 1.000000000000000000),
 ( 1.000000000000000000, 0.8047712409910814380, 1.000000000000000000) ) ) 
 REPRESENTATION_ITEM ( '' )  SURFACE ( )  );
#12853 = CARTESIAN_POINT ( 'NONE',  ( -4.799145180956616130, 0.5093500532425063732, -8.124999998634409692 ) ) ;
#12854 = CARTESIAN_POINT ( 'NONE',  ( -1.261996585732579224, 4.276409079477648589, 0.6875000013655923059 ) ) ;
#12855 = AXIS2_PLACEMENT_3D ( 'NONE', #6694, #9042, #4341 ) ;
#12856 = ORIENTED_EDGE ( 'NONE', *, *, #120, .F. ) ;
#12857 = CIRCLE ( 'NONE', #3566, 5.000000000000000888 ) ;
#12858 = ORIENTED_EDGE ( 'NONE', *, *, #8902, .T. ) ;
#12859 = DIRECTION ( 'NONE',  ( -0.000000000000000000, -0.000000000000000000, 1.000000000000000000 ) ) ;
#12860 = CARTESIAN_POINT ( 'NONE',  ( -4.458734125000001214, -28.87500000136559564, 1.846868145590734089 ) ) ;
#12861 = STYLED_ITEM ( 'NONE', ( #12149 ), #3386 ) ;
#12862 = EDGE_CURVE ( 'NONE', #15272, #13545, #8908, .T. ) ;
#12863 = VECTOR ( 'NONE', #8758, 1000.000000000000000 ) ;
#12864 = VERTEX_POINT ( 'NONE', #15458 ) ;
#12865 = VECTOR ( 'NONE', #7450, 1000.000000000000000 ) ;
#12866 = VECTOR ( 'NONE', #12981, 1000.000000000000000 ) ;
#12867 = DIRECTION ( 'NONE',  ( 0.000000000000000000, -0.000000000000000000, 1.000000000000000000 ) ) ;
#12868 = DIRECTION ( 'NONE',  ( -1.000000000000000000, 0.000000000000000000, 0.000000000000000000 ) ) ;
#12869 = CARTESIAN_POINT ( 'NONE',  ( 4.276409079477644148, 1.261996585732577891, 1.437500001365592972 ) ) ;
#12870 = CARTESIAN_POINT ( 'NONE',  ( -4.999999999999849898, 1.272547481429008309, -0.5865974826446477275 ) ) ;
#12871 = EDGE_CURVE ( 'NONE', #3920, #6708, #10993, .T. ) ;
#12872 = CARTESIAN_POINT ( 'NONE',  ( 2.500000000000000000, 2.357898499370433054, -1.951563910473907981E-15 ) ) ;
#12873 = CARTESIAN_POINT ( 'NONE',  ( 1.846868145590735200, -23.50000000136559564, -4.458734124999999437 ) ) ;
#12874 = ORIENTED_EDGE ( 'NONE', *, *, #13355, .T. ) ;
#12875 = CARTESIAN_POINT ( 'NONE',  ( 7.499999999999999112, 2.575910028905298077, -0.3641256808890091512 ) ) ;
#12876 = CARTESIAN_POINT ( 'NONE',  ( -7.500000000000007994, 4.330127018922187432, -7.564335161054492218 ) ) ;
#12877 = CARTESIAN_POINT ( 'NONE',  ( 4.403473400622098133, 6.117907484625860093, 1.852461055645154053E-15 ) ) ;
#12878 = EDGE_LOOP ( 'NONE', ( #14566, #11722, #9926, #6875, #2938 ) ) ;
#12879 = CARTESIAN_POINT ( 'NONE',  ( -4.204114297095464359, 1.660363174096617156, -3.602136431857887011 ) ) ;
#12880 = VERTEX_POINT ( 'NONE', #5668 ) ;
#12881 = ORIENTED_EDGE ( 'NONE', *, *, #4944, .F. ) ;
#12882 = AXIS2_PLACEMENT_3D ( 'NONE', #10858, #7076, #3116 ) ;
#12883 = CARTESIAN_POINT ( 'NONE',  ( -2.071067811865456854, -30.31249999999999645, 5.000000000000021316 ) ) ;
#12884 = CARTESIAN_POINT ( 'NONE',  ( -41.99999999999978684, -9.000000000000001776, -3.500000000000000888 ) ) ;
#12885 = CARTESIAN_POINT ( 'NONE',  ( -113.6871902368262965, -110.1917077999038099, -17.50000000000000000 ) ) ;
#12886 = DIRECTION ( 'NONE',  ( 0.000000000000000000, 0.000000000000000000, 1.000000000000000000 ) ) ;
#12887 = CYLINDRICAL_SURFACE ( 'NONE', #12180, 2.000000000000001776 ) ;
#12888 = CYLINDRICAL_SURFACE ( 'NONE', #14432, 32.00000000000000711 ) ;
#12889 = VECTOR ( 'NONE', #9175, 1000.000000000000000 ) ;
#12890 = CARTESIAN_POINT ( 'NONE',  ( 3.750000000000004441, -6.495190528383289141, 0.000000000000000000 ) ) ;
#12891 = LINE ( 'NONE', #11839, #2149 ) ;
#12892 = ADVANCED_FACE ( 'NONE', ( #5901 ), #4380, .F. ) ;
#12893 = CARTESIAN_POINT ( 'NONE',  ( 3.535533905932738197, -25.00000000273118417, -3.535533905932738197 ) ) ;
#12894 = EDGE_CURVE ( 'NONE', #11646, #15384, #7650, .T. ) ;
#12895 = CARTESIAN_POINT ( 'NONE',  ( -3.152801135295367096, -23.06250000136559564, -3.152801135295367541 ) ) ;
#12896 = CARTESIAN_POINT ( 'NONE',  ( 3.033343224707661712, -3.753672977998669946, -4.749999998634407028 ) ) ;
#12897 = ORIENTED_EDGE ( 'NONE', *, *, #2316, .T. ) ;
#12898 = LINE ( 'NONE', #5557, #13548 ) ;
#12899 = ORIENTED_EDGE ( 'NONE', *, *, #5413, .F. ) ;
#12900 = EDGE_LOOP ( 'NONE', ( #12672, #2940, #2891, #14949 ) ) ;
#12901 = CARTESIAN_POINT ( 'NONE',  ( -1.846868145590734756, -29.37500000136559564, -4.458734125000000326 ) ) ;
#12902 = LINE ( 'NONE', #720, #15135 ) ;
#12903 = ORIENTED_EDGE ( 'NONE', *, *, #7781, .T. ) ;
#12904 = CARTESIAN_POINT ( 'NONE',  ( 57.73502691896258199, 88.59290746114278647, 2.081668171172168513E-14 ) ) ;
#12905 = CARTESIAN_POINT ( 'NONE',  ( 7.500000000000000000, -1.645076096008604383, -7.030022527230893381 ) ) ;
#12906 = CARTESIAN_POINT ( 'NONE',  ( 1.261996585732578113, -4.276409079477644148, -3.562499998634407916 ) ) ;
#12907 = DIRECTION ( 'NONE',  ( 0.000000000000000000, 0.000000000000000000, -1.000000000000000000 ) ) ;
#12908 = CARTESIAN_POINT ( 'NONE',  ( 3.061616997868383141E-16, -26.75000000000000000, -5.000000000000000000 ) ) ;
#12909 = CARTESIAN_POINT ( 'NONE',  ( -1.261996585732579224, 4.276409079477648589, -7.062499998634407916 ) ) ;
#12910 = CYLINDRICAL_SURFACE ( 'NONE', #6283, 2.649999999999992806 ) ;
#12911 = LINE ( 'NONE', #15522, #10536 ) ;
#12912 = EDGE_CURVE ( 'NONE', #2474, #8373, #9693, .T. ) ;
#12913 = CARTESIAN_POINT ( 'NONE',  ( 5.000000000000000000, -24.12500000273118772, 0.000000000000000000 ) ) ;
#12914 = VERTEX_POINT ( 'NONE', #4451 ) ;
#12915 = CARTESIAN_POINT ( 'NONE',  ( -8.190561711645485556E-16, -26.68750000136559564, 4.458734124999999437 ) ) ;
#12916 = CARTESIAN_POINT ( 'NONE',  ( 2.390265326283148806, 4.391654775818395251, -6.875000000000002665 ) ) ;
#12917 = VERTEX_POINT ( 'NONE', #9233 ) ;
#12918 = VERTEX_POINT ( 'NONE', #8105 ) ;
#12919 = CARTESIAN_POINT ( 'NONE',  ( 0.000000000000000000, -2.357898499370432610, 3.252606517456513302E-15 ) ) ;
#12920 = EDGE_LOOP ( 'NONE', ( #11781, #7488 ) ) ;
#12921 = CARTESIAN_POINT ( 'NONE',  ( -28.86751345948196601, 1.999999999999998224, -75.00199999999976797 ) ) ;
#12922 = ORIENTED_EDGE ( 'NONE', *, *, #5940, .F. ) ;
#12923 = DIRECTION ( 'NONE',  ( 1.114413700119375779E-16, -0.000000000000000000, -1.000000000000000000 ) ) ;
#12924 = CARTESIAN_POINT ( 'NONE',  ( 40.04621312669365807, -3.477892933143086562, -27.97002203198492865 ) ) ;
#12925 = CARTESIAN_POINT ( 'NONE',  ( -8.190561711645485556E-16, -25.93750000136559564, 4.458734124999999437 ) ) ;
#12926 = CARTESIAN_POINT ( 'NONE',  ( 10.00000000000098765, -13.00000000000000178, 17.32050807568871065 ) ) ;
#12927 = EDGE_CURVE ( 'NONE', #4347, #10581, #15690, .T. ) ;
#12928 = CARTESIAN_POINT ( 'NONE',  ( -4.795541693661363958, -1.415196051561583790, -4.500000000000000888 ) ) ;
#12929 = EDGE_CURVE ( 'NONE', #15266, #13331, #2983, .T. ) ;
#12930 = APPLICATION_PROTOCOL_DEFINITION ( 'draft international standard', 'automotive_design', 1998, #4442 ) ;
#12931 = ADVANCED_FACE ( 'NONE', ( #1857 ), #5588, .T. ) ;
#12932 = CARTESIAN_POINT ( 'NONE',  ( 3.535533905932738197, -31.87500000000000000, -3.535533905932738197 ) ) ;
#12933 = CARTESIAN_POINT ( 'NONE',  ( 4.769696007084728073, -20.00000000000000000, 1.500000000000000000 ) ) ;
#12934 = EDGE_LOOP ( 'NONE', ( #9268, #13629, #11407, #7095 ) ) ;
#12935 = ORIENTED_EDGE ( 'NONE', *, *, #5062, .F. ) ;
#12936 = CARTESIAN_POINT ( 'NONE',  ( -7.298354728638057232, 4.926141412640825834, -7.913704048099944544 ) ) ;
#12937 = ORIENTED_EDGE ( 'NONE', *, *, #3213, .F. ) ;
#12938 = CARTESIAN_POINT ( 'NONE',  ( -4.391654775818395251, 2.390265326283148806, -4.625000000000000888 ) ) ;
#12939 = PRODUCT_DEFINITION_SHAPE ( 'NONE', 'NONE',  #15980 ) ;
#12940 = CIRCLE ( 'NONE', #8325, 2.055000000000000160 ) ;
#12941 =( BOUNDED_CURVE ( )  B_SPLINE_CURVE ( 2, ( #3106, #5684, #12938, #7877, #1874, #3176, #15478, #1801, #11647, #10456, #5446 ),
 .UNSPECIFIED., .F., .F. ) 
 B_SPLINE_CURVE_WITH_KNOTS ( ( 3, 2, 2, 2, 2, 3 ),
 ( 0.6545872658012773515, 0.6624999999999999778, 0.6750000000000000444, 0.6875000000000000000, 0.6999999999999999556, 0.7045872658012772849 ),
 .UNSPECIFIED. ) 
 CURVE ( )  GEOMETRIC_REPRESENTATION_ITEM ( )  RATIONAL_B_SPLINE_CURVE ( ( 0.9646335149384803742, 0.9518143178943441196, 1.000000000000000000, 0.9238795325112867385, 1.000000000000000000, 0.9238795325112867385, 1.000000000000000000, 0.9238795325112867385, 1.000000000000000000, 0.9720652146169428409, 0.9646335149384808183 ) ) 
 REPRESENTATION_ITEM ( '' )  );
#12942 = CARTESIAN_POINT ( 'NONE',  ( 4.999999999999849010, -1.272547481429013416, -2.961597479913464781 ) ) ;
#12943 = DIRECTION ( 'NONE',  ( -0.000000000000000000, -1.000000000000000000, -0.000000000000000000 ) ) ;
#12944 = EDGE_CURVE ( 'NONE', #3371, #11193, #4924, .T. ) ;
#12945 = CARTESIAN_POINT ( 'NONE',  ( 5.381735091635035495, -0.5711823568785978633, -6.937499997268816720 ) ) ;
#12946 = FILL_AREA_STYLE_COLOUR ( '', #11879 ) ;
#12947 = CARTESIAN_POINT ( 'NONE',  ( 4.209348295687701302, 3.401574460001766109, -1.937500000000002665 ) ) ;
#12948 = CARTESIAN_POINT ( 'NONE',  ( 19.99999999999956657, -8.786575603324269439E-13, 1.500000000000000000 ) ) ;
#12949 = ORIENTED_EDGE ( 'NONE', *, *, #11111, .F. ) ;
#12950 = CARTESIAN_POINT ( 'NONE',  ( 7.500000000000001776, 0.000000000000000000, 0.000000000000000000 ) ) ;
#12951 = DIRECTION ( 'NONE',  ( 0.000000000000000000, 0.000000000000000000, 1.000000000000000000 ) ) ;
#12952 = ITEM_DEFINED_TRANSFORMATION ( 'NONE', 'NONE', #385,  #3223 ) ;
#12953 = EDGE_LOOP ( 'NONE', ( #9147, #9788, #6352, #13936 ) ) ;
#12954 = DIRECTION ( 'NONE',  ( 0.005931855436079607087, -0.9999824063907751803, 0.000000000000000000 ) ) ;
#12955 = ORIENTED_EDGE ( 'NONE', *, *, #11241, .F. ) ;
#12956 = ORIENTED_EDGE ( 'NONE', *, *, #11162, .T. ) ;
#12957 = CARTESIAN_POINT ( 'NONE',  ( 5.000000000000000000, -23.12500000273118772, 0.000000000000000000 ) ) ;
#12958 = CARTESIAN_POINT ( 'NONE',  ( -39.99999999999999289, -11.00000000000000178, 8.300651832549021947E-13 ) ) ;
#12959 = VECTOR ( 'NONE', #4167, 1000.000000000000000 ) ;
#12960 = CARTESIAN_POINT ( 'NONE',  ( -7.500000000000005329, 3.988838049906425987, -0.8529248949437673311 ) ) ;
#12961 = CARTESIAN_POINT ( 'NONE',  ( -5.000000000000003553, -1.404940523648820476E-14, -8.420263044861757251 ) ) ;
#12962 = CARTESIAN_POINT ( 'NONE',  ( 14.41154273188013590, -35.00000000000000000, -60.96152422706631313 ) ) ;
#12963 = CARTESIAN_POINT ( 'NONE',  ( 2.071067811865476394, -23.18749999999999645, 5.000000000000000000 ) ) ;
#12964 = VECTOR ( 'NONE', #5253, 1000.000000000000000 ) ;
#12965 = DIRECTION ( 'NONE',  ( 0.000000000000000000, 0.000000000000000000, 1.000000000000000000 ) ) ;
#12966 = CARTESIAN_POINT ( 'NONE',  ( -43.99999999999978684, -11.00000000000000178, -1.500000000000000666 ) ) ;
#12967 = AXIS2_PLACEMENT_3D ( 'NONE', #5248, #7603, #12665 ) ;
#12968 = CARTESIAN_POINT ( 'NONE',  ( 5.000000000000004441, -2.247904837838113790E-16, -2.920263044861759472 ) ) ;
#12969 = CARTESIAN_POINT ( 'NONE',  ( -4.458734125000000326, -29.12500000136559564, 1.846868145590734089 ) ) ;
#12970 = CARTESIAN_POINT ( 'NONE',  ( -0.5093500532425060401, -4.799145180956616130, -0.6249999986344055847 ) ) ;
#12971 = ORIENTED_EDGE ( 'NONE', *, *, #14506, .T. ) ;
#12972 = CARTESIAN_POINT ( 'NONE',  ( -67.50000000000000000, 40.00000000000000000, -7.070249711157346244E-13 ) ) ;
#12973 = ORIENTED_EDGE ( 'NONE', *, *, #7419, .T. ) ;
#12974 = VERTEX_POINT ( 'NONE', #2480 ) ;
#12975 =( NAMED_UNIT ( * ) SI_UNIT ( $, .STERADIAN. ) SOLID_ANGLE_UNIT ( ) );
#12976 = PRODUCT_DEFINITION_SHAPE ( 'NONE', 'NONE',  #8905 ) ;
#12977 = CARTESIAN_POINT ( 'NONE',  ( 4.458734124999999437, -25.68750000136559564, 0.000000000000000000 ) ) ;
#12978 = CARTESIAN_POINT ( 'NONE',  ( 2.000000000000005329, -3.464101615137751722, 0.000000000000000000 ) ) ;
#12979 = CARTESIAN_POINT ( 'NONE',  ( 3.401574460001763445, -4.209348295687703079, -6.187500000000002665 ) ) ;
#12980 = EDGE_CURVE ( 'NONE', #9361, #11302, #12179, .T. ) ;
#12981 = DIRECTION ( 'NONE',  ( -1.000000000000000000, -0.000000000000000000, -3.343241100358131282E-16 ) ) ;
#12982 = CARTESIAN_POINT ( 'NONE',  ( -3.753672977998669502, -3.033343224707661712, -6.749999998634408804 ) ) ;
#12983 = CARTESIAN_POINT ( 'NONE',  ( 57.73502691896258199, -37.00000000000000711, 2.081668171172168513E-14 ) ) ;
#12984 = CARTESIAN_POINT ( 'NONE',  ( 5.000000000000000000, -26.00000000000000355, 0.000000000000000000 ) ) ;
#12985 = CARTESIAN_POINT ( 'NONE',  ( 4.276409079477644148, 1.261996585732577891, -7.312499998634407916 ) ) ;
#12986 = CARTESIAN_POINT ( 'NONE',  ( 0.000000000000000000, 0.000000000000000000, -4.484454397937119197 ) ) ;
#12987 = DIRECTION ( 'NONE',  ( -0.4999999999999998335, -0.000000000000000000, -0.8660254037844387076 ) ) ;
#12988 = CARTESIAN_POINT ( 'NONE',  ( 4.458734125000000326, -29.37500000136559208, -1.846868145590734978 ) ) ;
#12989 = EDGE_LOOP ( 'NONE', ( #14033, #9396 ) ) ;
#12990 = CARTESIAN_POINT ( 'NONE',  ( 1.846868145590735200, -28.25000000136559919, -4.458734124999999437 ) ) ;
#12991 = APPLICATION_CONTEXT ( 'automotive_design' ) ;
#12992 = CARTESIAN_POINT ( 'NONE',  ( -4.391654775818395251, 2.390265326283148806, -6.625000000000002665 ) ) ;
#12993 = VERTEX_POINT ( 'NONE', #7278 ) ;
#12994 = ORIENTED_EDGE ( 'NONE', *, *, #5718, .F. ) ;
#12995 = DIRECTION ( 'NONE',  ( 0.000000000000000000, -0.5000000000000011102, -0.8660254037844379305 ) ) ;
#12996 = MECHANICAL_DESIGN_GEOMETRIC_PRESENTATION_REPRESENTATION (  '', ( #3967 ), #4492 ) ;
#12997 = DIRECTION ( 'NONE',  ( 0.8660254037844381525, 0.000000000000000000, 0.5000000000000007772 ) ) ;
#12998 = ORIENTED_EDGE ( 'NONE', *, *, #4381, .F. ) ;
#12999 = DIRECTION ( 'NONE',  ( 1.000000000000000000, 0.000000000000000000, 0.000000000000000000 ) ) ;
#13000 = EDGE_CURVE ( 'NONE', #3510, #4663, #7354, .T. ) ;
#13001 = ADVANCED_FACE ( 'NONE', ( #7521 ), #7206, .T. ) ;
#13002 = CARTESIAN_POINT ( 'NONE',  ( -81.33974596215558961, -99.99999999999995737, -7.500000000000000000 ) ) ;
#13003 = CARTESIAN_POINT ( 'NONE',  ( -4.458734125000000326, -29.25000000136559564, -1.846868145590735644 ) ) ;
#13004 = DIRECTION ( 'NONE',  ( 0.000000000000000000, 0.000000000000000000, 1.000000000000000000 ) ) ;
#13005 = CARTESIAN_POINT ( 'NONE',  ( 2.500000000000000000, 2.357898499370433054, -1.951563910473907981E-15 ) ) ;
#13006 = APPLICATION_PROTOCOL_DEFINITION ( 'draft international standard', 'automotive_design', 1998, #2873 ) ;
#13007 = CIRCLE ( 'NONE', #9191, 2.500000000000909495 ) ;
#13008 = CARTESIAN_POINT ( 'NONE',  ( 0.6250000000000000000, -8.299410119600885594, -7.298562697733111726 ) ) ;
#13009 = DIRECTION ( 'NONE',  ( 0.000000000000000000, 0.000000000000000000, -1.000000000000000000 ) ) ;
#13010 = ORIENTED_EDGE ( 'NONE', *, *, #534, .F. ) ;
#13011 = VERTEX_POINT ( 'NONE', #10831 ) ;
#13012 = DIRECTION ( 'NONE',  ( 1.000000000000000000, 0.000000000000000000, 0.000000000000000000 ) ) ;
#13013 = VECTOR ( 'NONE', #14999, 1000.000000000000000 ) ;
#13014 = ORIENTED_EDGE ( 'NONE', *, *, #781, .F. ) ;
#13015 = ADVANCED_FACE ( 'NONE', ( #2253 ), #13463, .F. ) ;
#13016 = EDGE_CURVE ( 'NONE', #7869, #15369, #8174, .T. ) ;
#13017 = VECTOR ( 'NONE', #5153, 1000.000000000000000 ) ;
#13018 = DIRECTION ( 'NONE',  ( 0.000000000000000000, 0.000000000000000000, 1.000000000000000000 ) ) ;
#13019 = CARTESIAN_POINT ( 'NONE',  ( 1.828356344711641102, 3.563200125723180900, -5.433716356636336675E-16 ) ) ;
#13020 = CARTESIAN_POINT ( 'NONE',  ( 0.3208286057739604957, -4.433571671609698228, -0.3503314178412692548 ) ) ;
#13021 = STYLED_ITEM ( 'NONE', ( #13833 ), #1740 ) ;
#13022 = VECTOR ( 'NONE', #4232, 1000.000000000000000 ) ;
#13023 = CARTESIAN_POINT ( 'NONE',  ( 2.131511515620586383, 3.916244202832140253, 0.5625000013655921949 ) ) ;
#13024 = SURFACE_STYLE_FILL_AREA ( #11731 ) ;
#13025 = DIRECTION ( 'NONE',  ( 0.000000000000000000, -1.000000000000000000, 0.000000000000000000 ) ) ;
#13026 = CARTESIAN_POINT ( 'NONE',  ( 2.071067811865475505, -24.81250000000000000, -5.000000000000000888 ) ) ;
#13027 = ORIENTED_EDGE ( 'NONE', *, *, #11532, .T. ) ;
#13028 = AXIS2_PLACEMENT_3D ( 'NONE', #10060, #14989, #6262 ) ;
#13029 = CARTESIAN_POINT ( 'NONE',  ( 4.420982230657666712, -0.5789871446316176007, -0.3789984458506777676 ) ) ;
#13030 = CARTESIAN_POINT ( 'NONE',  ( 5.000000000000000888, 4.250000000000000000, 0.000000000000000000 ) ) ;
#13031 = ORIENTED_EDGE ( 'NONE', *, *, #7136, .F. ) ;
#13032 = ORIENTED_EDGE ( 'NONE', *, *, #3255, .F. ) ;
#13033 = ORIENTED_EDGE ( 'NONE', *, *, #15137, .F. ) ;
#13034 = CARTESIAN_POINT ( 'NONE',  ( 1.402244460665939663, 4.313165601266486959, -0.4094021847041934281 ) ) ;
#13035 = ADVANCED_FACE ( 'NONE', ( #12345 ), #9607, .F. ) ;
#13036 = CARTESIAN_POINT ( 'NONE',  ( -5.000000000000000888, 6.123233995736767268E-16, -25.03750572909317285 ) ) ;
#13037 =( BOUNDED_CURVE ( )  B_SPLINE_CURVE ( 2, ( #6468, #7771, #11380, #331, #10180, #12662, #1602, #14218, #9211 ),
 .UNSPECIFIED., .F., .F. ) 
 B_SPLINE_CURVE_WITH_KNOTS ( ( 3, 2, 2, 2, 3 ),
 ( 0.3249999999999999556, 0.3374999999999999667, 0.3499999999999999778, 0.3624999999999999889, 0.3750000000000000000 ),
 .UNSPECIFIED. ) 
 CURVE ( )  GEOMETRIC_REPRESENTATION_ITEM ( )  RATIONAL_B_SPLINE_CURVE ( ( 1.000000000000000444, 0.9238795325112864054, 1.000000000000000000, 0.9238795325112867385, 1.000000000000000000, 0.9238795325112867385, 1.000000000000000000, 0.9238795325112867385, 1.000000000000000000 ) ) 
 REPRESENTATION_ITEM ( '' )  );
#13038 = EDGE_CURVE ( 'NONE', #9472, #4440, #4763, .T. ) ;
#13039 = CARTESIAN_POINT ( 'NONE',  ( -7.500000000000005329, 1.854554393013823077, -0.1880126015361750780 ) ) ;
#13040 = AXIS2_PLACEMENT_3D ( 'NONE', #1297, #13330, #6243 ) ;
#13041 = CIRCLE ( 'NONE', #3253, 2.649999999999992806 ) ;
#13042 = FACE_OUTER_BOUND ( 'NONE', #6398, .T. ) ;
#13043 = CARTESIAN_POINT ( 'NONE',  ( 19.99999999999956657, -8.786575603324269439E-13, -11.50000000000000000 ) ) ;
#13044 = CARTESIAN_POINT ( 'NONE',  ( 5.000000000000000000, -23.00000000000000000, 0.000000000000000000 ) ) ;
#13045 = LINE ( 'NONE', #1985, #11031 ) ;
#13046 = DIRECTION ( 'NONE',  ( -1.000000000000000000, 0.000000000000000000, 1.239088197126290570E-16 ) ) ;
#13047 = DIRECTION ( 'NONE',  ( -1.000000000000000000, -0.000000000000000000, -0.000000000000000000 ) ) ;
#13048 = CARTESIAN_POINT ( 'NONE',  ( -1.846868145590737420, -28.00000000136559564, 4.458734124999997661 ) ) ;
#13049 = CARTESIAN_POINT ( 'NONE',  ( 3.916244202832140253, -2.131511515620588160, -1.437499998634406140 ) ) ;
#13050 = VERTEX_POINT ( 'NONE', #7 ) ;
#13051 = AXIS2_PLACEMENT_3D ( 'NONE', #12655, #13876, #14125 ) ;
#13052 = UNCERTAINTY_MEASURE_WITH_UNIT (LENGTH_MEASURE( 1.000000000000000082E-05 ), #5255, 'distance_accuracy_value', 'NONE');
#13053 = CARTESIAN_POINT ( 'NONE',  ( -21.01110699893041556, 0.000000000000000000, -39.04230484541333368 ) ) ;
#13054 = ORIENTED_EDGE ( 'NONE', *, *, #15417, .T. ) ;
#13055 = EDGE_LOOP ( 'NONE', ( #2222, #15210, #4917 ) ) ;
#13056 = CIRCLE ( 'NONE', #10498, 2.100000000000000089 ) ;
#13057 = SHAPE_REPRESENTATION_RELATIONSHIP ( 'NONE' , 'NONE' ,  #10906, #5806 ) ;
#13058 = VECTOR ( 'NONE', #8844, 1000.000000000000000 ) ;
#13059 = CARTESIAN_POINT ( 'NONE',  ( 4.458734125000000326, -26.62500000136559564, -1.846868145590734978 ) ) ;
#13060 = DIRECTION ( 'NONE',  ( 0.4999999999999960032, 0.8660254037844409281, 0.000000000000000000 ) ) ;
#13061 = EDGE_CURVE ( 'NONE', #11740, #8519, #5580, .T. ) ;
#13062 = LINE ( 'NONE', #8161, #1931 ) ;
#13063 = AXIS2_PLACEMENT_3D ( 'NONE', #15721, #13419, #9715 ) ;
#13064 = CARTESIAN_POINT ( 'NONE',  ( 2.500000000000000888, 3.061616997868384127E-16, -4.974599999999998801 ) ) ;
#13065 = CARTESIAN_POINT ( 'NONE',  ( -2.131511515620587272, -3.916244202832140253, -6.687499998634407028 ) ) ;
#13066 = CARTESIAN_POINT ( 'NONE',  ( 3.136976819694406782, -3.012271619929380417, 48.92291361451623999 ) ) ;
#13067 = AXIS2_PLACEMENT_3D ( 'NONE', #7898, #14019, #5387 ) ;
#13068 = CARTESIAN_POINT ( 'NONE',  ( -5.000000000000000888, -25.56250000000000355, -2.071067811865475949 ) ) ;
#13069 = AXIS2_PLACEMENT_3D ( 'NONE', #12717, #14018, #13937 ) ;
#13070 = CARTESIAN_POINT ( 'NONE',  ( 5.381735091635035495, -0.5711823568785978633, 0.9374999999999980016 ) ) ;
#13071 = PLANE ( 'NONE',  #9159 ) ;
#13072 = DIRECTION ( 'NONE',  ( -0.000000000000000000, -1.000000000000000000, -0.000000000000000000 ) ) ;
#13073 = CARTESIAN_POINT ( 'NONE',  ( 4.458734124999999437, -30.50000000136559919, 1.846868145590737864 ) ) ;
#13074 = ORIENTED_EDGE ( 'NONE', *, *, #934, .F. ) ;
#13075 = FACE_OUTER_BOUND ( 'NONE', #8356, .T. ) ;
#13076 = ADVANCED_FACE ( 'NONE', ( #8734 ), #12107, .F. ) ;
#13077 = CARTESIAN_POINT ( 'NONE',  ( -124.9999999999999716, -10.00000000000001066, 17.50000000000000000 ) ) ;
#13078 = ORIENTED_EDGE ( 'NONE', *, *, #7133, .F. ) ;
#13079 = VECTOR ( 'NONE', #13527, 1000.000000000000000 ) ;
#13080 = EDGE_LOOP ( 'NONE', ( #15750, #8455, #14321, #9901, #2207 ) ) ;
#13081 = CARTESIAN_POINT ( 'NONE',  ( -5.000000000000004441, -7.530481206757679743E-15, -3.420263044861759916 ) ) ;
#13082 = CARTESIAN_POINT ( 'NONE',  ( 2.071067811865497710, -29.31250000273118062, 4.999999999999978684 ) ) ;
#13083 = DIRECTION ( 'NONE',  ( 0.000000000000000000, 1.000000000000000000, 0.000000000000000000 ) ) ;
#13084 = EDGE_LOOP ( 'NONE', ( #5499, #13032, #11394, #11338, #15301, #4015 ) ) ;
#13085 = DIRECTION ( 'NONE',  ( 0.000000000000000000, 1.000000000000000000, 0.000000000000000000 ) ) ;
#13086 = VECTOR ( 'NONE', #1492, 1000.000000000000114 ) ;
#13087 = DIRECTION ( 'NONE',  ( -0.000000000000000000, 1.000000000000000000, -0.000000000000000000 ) ) ;
#13088 = CARTESIAN_POINT ( 'NONE',  ( 4.458734124999999437, -26.68750000136559564, 0.000000000000000000 ) ) ;
#13089 = LINE ( 'NONE', #8345, #582 ) ;
#13090 = APPLICATION_CONTEXT ( 'automotive_design' ) ;
#13091 = CARTESIAN_POINT ( 'NONE',  ( -2.390265326283148806, -4.391654775818394363, -0.2499999972688168870 ) ) ;
#13092 = CARTESIAN_POINT ( 'NONE',  ( 5.000000000000000888, -30.93750000000000355, -2.071067811865475505 ) ) ;
#13093 = CIRCLE ( 'NONE', #2252, 2.649999999999992806 ) ;
#13094 = CARTESIAN_POINT ( 'NONE',  ( 4.197393957002303999, -0.4069871074557456780, -3.503767560748925813 ) ) ;
#13095 = ADVANCED_FACE ( 'NONE', ( #14625 ), #13546, .F. ) ;
#13097 = EDGE_CURVE ( 'NONE', #1597, #13901, #80, .T. ) ;
#13096 = ORIENTED_EDGE ( 'NONE', *, *, #4546, .T. ) ;
#13098 = AXIS2_PLACEMENT_3D ( 'NONE', #13781, #11369, #320 ) ;
#13099 = VERTEX_POINT ( 'NONE', #9927 ) ;
#13100 = VERTEX_POINT ( 'NONE', #1200 ) ;
#13101 = AXIS2_PLACEMENT_3D ( 'NONE', #6848, #5780, #10721 ) ;
#13102 = VECTOR ( 'NONE', #5030, 1000.000000000000000 ) ;
#13103 = DIRECTION ( 'NONE',  ( 1.000000000000000000, 0.000000000000000000, 0.000000000000000000 ) ) ;
#13104 = CARTESIAN_POINT ( 'NONE',  ( 0.5093500532425063732, 4.799145180956616130, -0.1249999986344088321 ) ) ;
#13105 = DIRECTION ( 'NONE',  ( 1.000000000000000000, -6.123233995736766036E-17, -6.123233995736764803E-17 ) ) ;
#13106 = PRODUCT ( 'socket head cap screw_iso_ISO 4762 M5 x 12 - 12N', 'socket head cap screw_iso_ISO 4762 M5 x 12 - 12N', '', ( #7714 ) ) ;
#13107 = CARTESIAN_POINT ( 'NONE',  ( -1.415196051561583790, 4.795541693661363958, -6.624999997268815832 ) ) ;
#13108 = LINE ( 'NONE', #6752, #3105 ) ;
#13109 = LINE ( 'NONE', #14638, #7359 ) ;
#13110 = EDGE_CURVE ( 'NONE', #14412, #2071, #12519, .T. ) ;
#13111 = ORIENTED_EDGE ( 'NONE', *, *, #15393, .F. ) ;
#13112 = CARTESIAN_POINT ( 'NONE',  ( 5.000000000000000888, 0.000000000000000000, -25.03750572909317285 ) ) ;
#13113 = CARTESIAN_POINT ( 'NONE',  ( 5.000000000000092371, 0.7223674278660651149, -2.896799362785969834 ) ) ;
#13114 = AXIS2_PLACEMENT_3D ( 'NONE', #1959, #11887, #9482 ) ;
#13115 =( NAMED_UNIT ( * ) PLANE_ANGLE_UNIT ( ) SI_UNIT ( $, .RADIAN. ) );
#13116 = ORIENTED_EDGE ( 'NONE', *, *, #3425, .T. ) ;
#13117 = CYLINDRICAL_SURFACE ( 'NONE', #9543, 9.999999999999992895 ) ;
#13118 = VERTEX_POINT ( 'NONE', #13395 ) ;
#13119 = VERTEX_POINT ( 'NONE', #13638 ) ;
#13120 = CARTESIAN_POINT ( 'NONE',  ( -28.86751345948126612, -3.000000000000000000, -22.00000000000000711 ) ) ;
#13121 = CARTESIAN_POINT ( 'NONE',  ( -94.14213562373093680, -30.85786437626904899, -17.49999999999999645 ) ) ;
#13122 = VECTOR ( 'NONE', #7505, 1000.000000000000000 ) ;
#13123 = AXIS2_PLACEMENT_3D ( 'NONE', #14958, #5329, #2483 ) ;
#13124 = CARTESIAN_POINT ( 'NONE',  ( -7.500000000000005329, 4.330127018922194537, -0.9999999999999974465 ) ) ;
#13125 = CARTESIAN_POINT ( 'NONE',  ( 4.391654775818395251, -2.390265326283149694, -5.125000000000000888 ) ) ;
#13126 = DIRECTION ( 'NONE',  ( 0.000000000000000000, 0.000000000000000000, 1.000000000000000000 ) ) ;
#13127 = CARTESIAN_POINT ( 'NONE',  ( 47.32050807568879947, -4.999999999999997335, -41.96152422706630603 ) ) ;
#13128 = DIRECTION ( 'NONE',  ( -1.319090325525611458E-16, -1.000000000000000000, 0.000000000000000000 ) ) ;
#13129 = DIRECTION ( 'NONE',  ( 0.000000000000000000, 0.000000000000000000, 1.000000000000000000 ) ) ;
#13130 = ADVANCED_FACE ( 'NONE', ( #2333, #4849, #9772 ), #6145, .T. ) ;
#13131 = DIRECTION ( 'NONE',  ( -0.000000000000000000, 1.000000000000000000, -0.000000000000000000 ) ) ;
#13132 = EDGE_CURVE ( 'NONE', #1169, #15878, #2685, .T. ) ;
#13133 = CARTESIAN_POINT ( 'NONE',  ( 1.846868145590735200, -29.50000000136559564, -4.458734124999999437 ) ) ;
#13134 = ADVANCED_FACE ( 'NONE', ( #7843 ), #3872, .T. ) ;
#13135 = ADVANCED_FACE ( 'NONE', ( #2649 ), #8536, .F. ) ;
#13136 = CARTESIAN_POINT ( 'NONE',  ( -0.5093500532425060401, -4.799145180956616130, 0.3750000013655915843 ) ) ;
#13137 = EDGE_LOOP ( 'NONE', ( #288, #11554 ) ) ;
#13138 = AXIS2_PLACEMENT_3D ( 'NONE', #13584, #6091, #8601 ) ;
#13139 = CARTESIAN_POINT ( 'NONE',  ( 7.847095227763521308, 4.129731495738486302, -7.493596212620240671 ) ) ;
#13140 = ORIENTED_EDGE ( 'NONE', *, *, #2709, .F. ) ;
#13141 = VERTEX_POINT ( 'NONE', #11537 ) ;
#13142 =( BOUNDED_CURVE ( )  B_SPLINE_CURVE ( 2, ( #6766, #2062, #13125, #10330, #3281, #4489, #10640, #8144, #4414, #8227, #11600 ),
 .UNSPECIFIED., .F., .F. ) 
 B_SPLINE_CURVE_WITH_KNOTS ( ( 3, 2, 2, 2, 2, 3 ),
 ( 0.7045872658012772849, 0.7125000000000000222, 0.7249999999999999778, 0.7375000000000000444, 0.7500000000000000000, 0.7545872658012773293 ),
 .UNSPECIFIED. ) 
 CURVE ( )  GEOMETRIC_REPRESENTATION_ITEM ( )  RATIONAL_B_SPLINE_CURVE ( ( 0.9646335149384808183, 0.9518143178943441196, 1.000000000000000000, 0.9238795325112867385, 1.000000000000000000, 0.9238795325112867385, 1.000000000000000000, 0.9238795325112867385, 1.000000000000000000, 0.9720652146169423968, 0.9646335149384803742 ) ) 
 REPRESENTATION_ITEM ( '' )  );
#13143 = CARTESIAN_POINT ( 'NONE',  ( 1.846868145590736310, -26.87500000136559208, 4.458734124999999437 ) ) ;
#13144 = CARTESIAN_POINT ( 'NONE',  ( 3.355112389629172576, -2.681727112203168950, -0.2256878752776777242 ) ) ;
#13145 = FACE_OUTER_BOUND ( 'NONE', #2293, .T. ) ;
#13146 = CARTESIAN_POINT ( 'NONE',  ( -2.071067811865499486, -29.68750000000000000, -4.999999999999975131 ) ) ;
#13147 = CARTESIAN_POINT ( 'NONE',  ( -2.131511515620587272, -3.916244202832140253, -3.687499998634407916 ) ) ;
#13148 = CARTESIAN_POINT ( 'NONE',  ( 4.795541693661363958, 1.415196051561583790, -5.874999997268814944 ) ) ;
#13149 = CARTESIAN_POINT ( 'NONE',  ( -5.000000000000000888, -26.43750000000000355, 2.071067811865474617 ) ) ;
#13150 = CARTESIAN_POINT ( 'NONE',  ( 4.276409079477644148, 1.261996585732577891, -8.312499998634407916 ) ) ;
#13151 = DIRECTION ( 'NONE',  ( -0.000000000000000000, -1.000000000000000000, -0.000000000000000000 ) ) ;
#13152 = CARTESIAN_POINT ( 'NONE',  ( -21.01110699893041911, 0.000000000000000000, -36.39230484541334221 ) ) ;
#13153 = CARTESIAN_POINT ( 'NONE',  ( -1.846868145590734756, -31.12500000136559564, -4.458734125000000326 ) ) ;
#13154 = ADVANCED_FACE ( 'NONE', ( #15192 ), #13883, .F. ) ;
#13155 = VERTEX_POINT ( 'NONE', #15273 ) ;
#13156 = CARTESIAN_POINT ( 'NONE',  ( 1.846868145590735200, -24.25000000136559564, -4.458734124999999437 ) ) ;
#13157 = DIRECTION ( 'NONE',  ( -0.000000000000000000, -1.000000000000000000, -0.000000000000000000 ) ) ;
#13158 = ORIENTED_EDGE ( 'NONE', *, *, #11649, .F. ) ;
#13159 = EDGE_LOOP ( 'NONE', ( #13116, #1614, #6280, #9293 ) ) ;
#13160 = CARTESIAN_POINT ( 'NONE',  ( 0.5711823568785988625, 5.381735091635026613, -3.687499997268817609 ) ) ;
#13161 = CARTESIAN_POINT ( 'NONE',  ( 2.730187237215162345E-16, -29.18750000136559208, -4.458734124999999437 ) ) ;
#13162 = CARTESIAN_POINT ( 'NONE',  ( 5.000000000000000000, -29.12500000273118772, 0.000000000000000000 ) ) ;
#13163 = ORIENTED_EDGE ( 'NONE', *, *, #13234, .F. ) ;
#13164 = CARTESIAN_POINT ( 'NONE',  ( 5.000000000000091482, 0.7223674278660408010, -0.02179936551715794604 ) ) ;
#13165 = FACE_OUTER_BOUND ( 'NONE', #5537, .T. ) ;
#13166 = DIRECTION ( 'NONE',  ( -0.000000000000000000, 0.000000000000000000, 1.000000000000000000 ) ) ;
#13167 = CARTESIAN_POINT ( 'NONE',  ( 1.846868145590736310, -26.87500000136559208, 4.458734124999999437 ) ) ;
#13168 = CARTESIAN_POINT ( 'NONE',  ( 5.000000000000004441, 3.034671531081452754E-15, -0.9202630448617579173 ) ) ;
#13169 = CARTESIAN_POINT ( 'NONE',  ( -0.5711823568785977523, -5.381735091635034607, -0.1874999972688185246 ) ) ;
#13170 = CARTESIAN_POINT ( 'NONE',  ( 5.000000000000000888, -31.06250000273118417, -2.071067811865475505 ) ) ;
#13171 = DIRECTION ( 'NONE',  ( 0.000000000000000000, -0.5000000000000011102, -0.8660254037844379305 ) ) ;
#13172 = EDGE_LOOP ( 'NONE', ( #11631, #11939, #12079, #7345 ) ) ;
#13173 = VERTEX_POINT ( 'NONE', #9133 ) ;
#13174 = CARTESIAN_POINT ( 'NONE',  ( 0.000000000000000000, -1.178949249685213863, 2.042000000000002924 ) ) ;
#13175 = ORIENTED_EDGE ( 'NONE', *, *, #5840, .T. ) ;
#13176 = DIRECTION ( 'NONE',  ( -0.000000000000000000, 0.000000000000000000, -1.000000000000000000 ) ) ;
#13177 = EDGE_CURVE ( 'NONE', #635, #9146, #2970, .T. ) ;
#13178 = CARTESIAN_POINT ( 'NONE',  ( 1.312671235360372224, 3.860931062424219462, -0.05923475698270440348 ) ) ;
#13179 = CARTESIAN_POINT ( 'NONE',  ( 3.916244202832140253, -2.131511515620588160, -0.4374999986344086933 ) ) ;
#13180 = DIRECTION ( 'NONE',  ( 6.123233995736766036E-17, 1.000000000000000000, 0.000000000000000000 ) ) ;
#13181 = CARTESIAN_POINT ( 'NONE',  ( 4.799145180956616130, -0.5093500532425063732, -0.6249999986344092484 ) ) ;
#13182 = PLANE ( 'NONE',  #2258 ) ;
#13183 = CARTESIAN_POINT ( 'NONE',  ( 5.000000000000000000, -22.12500000273118417, 0.000000000000000000 ) ) ;
#13184 = ORIENTED_EDGE ( 'NONE', *, *, #5019, .T. ) ;
#13185 = DIRECTION ( 'NONE',  ( 0.000000000000000000, -1.000000000000000000, 1.287488025362403787E-15 ) ) ;
#13186 = DIRECTION ( 'NONE',  ( -0.000000000000000000, -1.000000000000000000, -0.000000000000000000 ) ) ;
#13187 = ORIENTED_EDGE ( 'NONE', *, *, #15548, .F. ) ;
#13188 = CYLINDRICAL_SURFACE ( 'NONE', #12882, 9.999999999999994671 ) ;
#13189 = VERTEX_POINT ( 'NONE', #12822 ) ;
#13190 = VERTEX_POINT ( 'NONE', #6304 ) ;
#13191 = CARTESIAN_POINT ( 'NONE',  ( 2.500000000000000000, 1.178949249685213863, -2.042000000000001148 ) ) ;
#13192 = DIRECTION ( 'NONE',  ( -1.000000000000000000, 0.000000000000000000, -0.000000000000000000 ) ) ;
#13193 = CIRCLE ( 'NONE', #1333, 2.500000000000000888 ) ;
#13194 = LINE ( 'NONE', #3663, #13264 ) ;
#13195 = EDGE_CURVE ( 'NONE', #14177, #1787, #11220, .T. ) ;
#13196 = EDGE_CURVE ( 'NONE', #4698, #5290, #3958, .T. ) ;
#13197 = CARTESIAN_POINT ( 'NONE',  ( -7.914984360234578631, 3.818534719232089980, -7.907701344400643428 ) ) ;
#13198 = PLANE ( 'NONE',  #7805 ) ;
#13199 = CARTESIAN_POINT ( 'NONE',  ( -3.535533905932737309, -29.75000000273118417, -3.535533905932738197 ) ) ;
#13200 = CARTESIAN_POINT ( 'NONE',  ( 4.795541693661363958, 1.415196051561583790, -0.8749999972688139449 ) ) ;
#13201 = CARTESIAN_POINT ( 'NONE',  ( -1.154700538379222596, 88.59290746114278647, -34.00000000000000000 ) ) ;
#13202 = CARTESIAN_POINT ( 'NONE',  ( -1.846868145590737420, -30.00000000136559919, 4.458734124999997661 ) ) ;
#13203 = CARTESIAN_POINT ( 'NONE',  ( 0.5093500532425063732, 4.799145180956616130, -2.124999998634406584 ) ) ;
#13204 = EDGE_LOOP ( 'NONE', ( #3899, #2622, #10603, #249 ) ) ;
#13205 = CARTESIAN_POINT ( 'NONE',  ( 3.295171437449766927, 7.213553046161560012, -7.590212325761490852 ) ) ;
#13206 = ORIENTED_EDGE ( 'NONE', *, *, #7211, .F. ) ;
#13207 = ORIENTED_EDGE ( 'NONE', *, *, #4109, .F. ) ;
#13208 = ORIENTED_EDGE ( 'NONE', *, *, #7446, .T. ) ;
#13209 = CARTESIAN_POINT ( 'NONE',  ( 3.152801135295366208, -28.81250000136559564, 3.152801135295367985 ) ) ;
#13210 = CARTESIAN_POINT ( 'NONE',  ( -35.00000000000000000, 37.00000000000000000, 0.000000000000000000 ) ) ;
#13211 = DIRECTION ( 'NONE',  ( 0.000000000000000000, 0.000000000000000000, -1.000000000000000000 ) ) ;
#13212 = ADVANCED_FACE ( 'NONE', ( #255 ), #8972, .F. ) ;
#13213 = EDGE_CURVE ( 'NONE', #14496, #13118, #13037, .T. ) ;
#13214 = CIRCLE ( 'NONE', #6274, 25.00000000000000000 ) ;
#13215 = AXIS2_PLACEMENT_3D ( 'NONE', #15651, #5469, #9195 ) ;
#13216 = CARTESIAN_POINT ( 'NONE',  ( 12.67949192431126093, -37.00000000000000711, -61.96152422706632024 ) ) ;
#13217 = CARTESIAN_POINT ( 'NONE',  ( -1.415196051561583790, 4.795541693661363958, -5.624999997268814944 ) ) ;
#13218 = CARTESIAN_POINT ( 'NONE',  ( 3.061616997868383141E-16, -22.75000000000000000, -5.000000000000000000 ) ) ;
#13219 = CARTESIAN_POINT ( 'NONE',  ( 3.916244202832140253, -2.131511515620588160, -7.437499998634407916 ) ) ;
#13220 = CARTESIAN_POINT ( 'NONE',  ( 0.000000000000000000, 0.000000000000000000, 0.000000000000000000 ) ) ;
#13221 = CIRCLE ( 'NONE', #14045, 2.649999999999992806 ) ;
#13222 = CARTESIAN_POINT ( 'NONE',  ( -4.662883599861174844, -0.5303216768924871038, -0.2203019408131941803 ) ) ;
#13223 = CARTESIAN_POINT ( 'NONE',  ( 2.071067811865476394, -21.31250000273118772, 5.000000000000000000 ) ) ;
#13224 = EDGE_LOOP ( 'NONE', ( #10098, #3112 ) ) ;
#13225 = CIRCLE ( 'NONE', #8613, 9.999999999999994671 ) ;
#13226 = DIRECTION ( 'NONE',  ( 0.000000000000000000, 0.000000000000000000, -1.000000000000000000 ) ) ;
#13227 = ORIENTED_EDGE ( 'NONE', *, *, #13750, .T. ) ;
#13228 = ORIENTED_EDGE ( 'NONE', *, *, #13327, .F. ) ;
#13229 = CARTESIAN_POINT ( 'NONE',  ( 3.061616997868383141E-16, -27.87500000273118772, -5.000000000000000000 ) ) ;
#13230 = CARTESIAN_POINT ( 'NONE',  ( 2.730187237215162345E-16, -28.18750000136559564, -4.458734124999999437 ) ) ;
#13231 = CYLINDRICAL_SURFACE ( 'NONE', #4016, 3.499999999999999556 ) ;
#13232 = ORIENTED_EDGE ( 'NONE', *, *, #907, .T. ) ;
#13233 = DIRECTION ( 'NONE',  ( 0.000000000000000000, 0.000000000000000000, 1.000000000000000000 ) ) ;
#13234 = EDGE_CURVE ( 'NONE', #14535, #10378, #14369, .T. ) ;
#13235 = EDGE_CURVE ( 'NONE', #4642, #7472, #10503, .T. ) ;
#13236 = PRODUCT_DEFINITION_SHAPE ( 'NONE', 'NONE',  #15971 ) ;
#13237 = CARTESIAN_POINT ( 'NONE',  ( -3.096526599377910305, 6.872473572140717302, -4.269046054161672230E-16 ) ) ;
#13238 = B_SPLINE_CURVE_WITH_KNOTS ( 'NONE', 3,
 ( #9021, #13755, #6504, #13925 ),
 .UNSPECIFIED., .F., .F.,
 ( 4, 4 ),
 ( 8.125557066451241256E-17, 0.001452767664617488205 ),
 .UNSPECIFIED. ) ;
#13239 = CARTESIAN_POINT ( 'NONE',  ( -44.99999999999999289, -35.00000000000000000, 7.500000000000001776 ) ) ;
#13240 = CARTESIAN_POINT ( 'NONE',  ( 4.458734124999999437, -23.68750000136559564, 0.000000000000000000 ) ) ;
#13241 = CARTESIAN_POINT ( 'NONE',  ( 35.00000000000000000, 40.00000000000000000, -5.999999999999991118 ) ) ;
#13242 = DIRECTION ( 'NONE',  ( -1.114413700119375779E-16, -0.000000000000000000, 1.000000000000000000 ) ) ;
#13243 = CARTESIAN_POINT ( 'NONE',  ( -6.762176242291807225E-13, 50.00000000000000000, 64.84999999999932641 ) ) ;
#13244 = PLANE ( 'NONE',  #13335 ) ;
#13245 = ORIENTED_EDGE ( 'NONE', *, *, #1639, .T. ) ;
#13246 = EDGE_LOOP ( 'NONE', ( #15820, #4283, #3252, #2092 ) ) ;
#13247 = CARTESIAN_POINT ( 'NONE',  ( -5.088535779736633735, 5.722386535632430160, -7.491772860716511495 ) ) ;
#13248 = ORIENTED_EDGE ( 'NONE', *, *, #11048, .F. ) ;
#13249 = ADVANCED_FACE ( 'NONE', ( #8322 ), #10589, .T. ) ;
#13250 = CARTESIAN_POINT ( 'NONE',  ( -17.99999999999979394, -9.000000000000001776, 1.499999999999999112 ) ) ;
#13251 = DIRECTION ( 'NONE',  ( 0.000000000000000000, 0.000000000000000000, 1.000000000000000000 ) ) ;
#13252 = EDGE_LOOP ( 'NONE', ( #14591, #15307, #4520 ) ) ;
#13253 = CARTESIAN_POINT ( 'NONE',  ( 4.276409079477644148, 1.261996585732577891, -0.3124999986344085823 ) ) ;
#13254 = DIRECTION ( 'NONE',  ( -0.4999999999999919509, 0.000000000000000000, -0.8660254037844432595 ) ) ;
#13255 = CARTESIAN_POINT ( 'NONE',  ( -2.131511515620587272, -3.916244202832140253, -2.937499998634407472 ) ) ;
#13256 = DIRECTION ( 'NONE',  ( 0.000000000000000000, 0.000000000000000000, 1.000000000000000000 ) ) ;
#13257 = ORIENTED_EDGE ( 'NONE', *, *, #7728, .F. ) ;
#13258 = CARTESIAN_POINT ( 'NONE',  ( -5.000000000000000888, -22.43749999999999645, 2.071067811865474617 ) ) ;
#13259 = AXIS2_PLACEMENT_3D ( 'NONE', #11404, #277, #12287 ) ;
#13260 = EDGE_CURVE ( 'NONE', #7787, #13811, #6876, .T. ) ;
#13261 = VERTEX_POINT ( 'NONE', #9523 ) ;
#13262 = CARTESIAN_POINT ( 'NONE',  ( 17.00000000000000000, 2.789133085058097101E-16, -2.055000000000000160 ) ) ;
#13263 = VERTEX_POINT ( 'NONE', #4585 ) ;
#13264 = VECTOR ( 'NONE', #15964, 1000.000000000000000 ) ;
#13265 = EDGE_LOOP ( 'NONE', ( #13303, #4972 ) ) ;
#13266 = CARTESIAN_POINT ( 'NONE',  ( -3.916244202832140253, 2.131511515620587272, -2.187499998634407028 ) ) ;
#13267 = LINE ( 'NONE', #2210, #2191 ) ;
#13268 = TOROIDAL_SURFACE ( 'NONE', #14067, 28.00000000000000355, 2.000000000000000000 ) ;
#13269 = AXIS2_PLACEMENT_3D ( 'NONE', #12706, #7654, #1498 ) ;
#13270 = CARTESIAN_POINT ( 'NONE',  ( 4.795541693661363958, 1.415196051561583790, -8.874999997268814056 ) ) ;
#13271 = CARTESIAN_POINT ( 'NONE',  ( -2.390265326283148806, -4.391654775818394363, -2.375000000000002220 ) ) ;
#13272 = VECTOR ( 'NONE', #603, 1000.000000000000000 ) ;
#13273 = CARTESIAN_POINT ( 'NONE',  ( 3.061616997868383141E-16, -29.87500000273118417, -5.000000000000000000 ) ) ;
#13274 = DIRECTION ( 'NONE',  ( 1.000000000000000000, 0.000000000000000000, 0.000000000000000000 ) ) ;
#13275 = DIRECTION ( 'NONE',  ( 0.000000000000000000, 0.000000000000000000, -1.000000000000000000 ) ) ;
#13276 = CARTESIAN_POINT ( 'NONE',  ( 3.152801135295367541, -31.56250000136559564, -3.152801135295367541 ) ) ;
#13277 = CARTESIAN_POINT ( 'NONE',  ( -4.799145180956616130, 0.5093500532425063732, 0.1250000013655913900 ) ) ;
#13278 = ORIENTED_EDGE ( 'NONE', *, *, #15093, .T. ) ;
#13279 = DIRECTION ( 'NONE',  ( -0.000000000000000000, -1.000000000000000000, -0.000000000000000000 ) ) ;
#13280 = EDGE_CURVE ( 'NONE', #4993, #6462, #13041, .T. ) ;
#13281 = ORIENTED_EDGE ( 'NONE', *, *, #8396, .F. ) ;
#13282 = ORIENTED_EDGE ( 'NONE', *, *, #10199, .T. ) ;
#13283 = EDGE_CURVE ( 'NONE', #5750, #10008, #15125, .T. ) ;
#13284 = TOROIDAL_SURFACE ( 'NONE', #6342, 2.700000000000000622, 0.2000000000000000111 ) ;
#13285 = EDGE_LOOP ( 'NONE', ( #3247, #9286, #10112, #3865 ) ) ;
#13286 = CARTESIAN_POINT ( 'NONE',  ( -1.846868145590737420, -26.00000000136559564, 4.458734124999999437 ) ) ;
#13287 = CARTESIAN_POINT ( 'NONE',  ( 0.000000000000000000, 40.00000000000000000, 0.000000000000000000 ) ) ;
#13288 = VECTOR ( 'NONE', #5978, 1000.000000000000000 ) ;
#13289 = CARTESIAN_POINT ( 'NONE',  ( 3.535533905932738197, -30.00000000273118417, -3.535533905932738197 ) ) ;
#13290 = DIRECTION ( 'NONE',  ( 1.000000000000000000, 0.000000000000000000, 0.000000000000000000 ) ) ;
#13291 = CARTESIAN_POINT ( 'NONE',  ( 30.02221399786052913, 0.000000000000000000, 16.00000000000001066 ) ) ;
#13292 = CARTESIAN_POINT ( 'NONE',  ( -2.071067811865478170, -22.31250000000000000, 5.000000000000000000 ) ) ;
#13293 = AXIS2_PLACEMENT_3D ( 'NONE', #12229, #1168, #11040 ) ;
#13294 = CARTESIAN_POINT ( 'NONE',  ( -1.415196051561583790, 4.795541693661363958, -1.750000000000001554 ) ) ;
#13295 = DIRECTION ( 'NONE',  ( -0.000000000000000000, -1.000000000000000000, -0.000000000000000000 ) ) ;
#13296 = CARTESIAN_POINT ( 'NONE',  ( 47.32050807568875683, -35.00000000000000000, 41.96152422706633445 ) ) ;
#13297 = CARTESIAN_POINT ( 'NONE',  ( 5.000000000000000000, -21.12500000273118772, 0.000000000000000000 ) ) ;
#13298 = AXIS2_PLACEMENT_3D ( 'NONE', #165, #1354, #5081 ) ;
#13299 = CARTESIAN_POINT ( 'NONE',  ( 5.000000000000002665, 0.000000000000000000, -2.700000000000000622 ) ) ;
#13300 = ORIENTED_EDGE ( 'NONE', *, *, #13516, .F. ) ;
#13301 = CARTESIAN_POINT ( 'NONE',  ( 7.298354728637884925, -4.926141412640459905, -7.913704048099823751 ) ) ;
#13302 = ORIENTED_EDGE ( 'NONE', *, *, #9664, .F. ) ;
#13303 = ORIENTED_EDGE ( 'NONE', *, *, #3492, .T. ) ;
#13304 = ADVANCED_FACE ( 'NONE', ( #9441 ), #8083, .T. ) ;
#13305 = DIRECTION ( 'NONE',  ( 0.000000000000000000, 1.000000000000000000, 0.000000000000000000 ) ) ;
#13306 = CARTESIAN_POINT ( 'NONE',  ( 1.846868145590736310, -30.62500000136559208, 4.458734124999999437 ) ) ;
#13307 = LINE ( 'NONE', #9605, #5321 ) ;
#13308 = AXIS2_PLACEMENT_3D ( 'NONE', #5766, #15640, #11821 ) ;
#13309 = ORIENTED_EDGE ( 'NONE', *, *, #2867, .T. ) ;
#13310 = CARTESIAN_POINT ( 'NONE',  ( -116.3984487401935155, -110.2077908763549914, -7.500000000000000000 ) ) ;
#13311 = CIRCLE ( 'NONE', #14885, 2.649999999999985700 ) ;
#13312 = CLOSED_SHELL ( 'NONE', ( #12110, #14529, #11416, #13555, #10250, #6423, #9534, #7851, #12376, #870, #13249, #5844, #14445, #12300, #12140, #422, #1365, #2951, #9685, #12416, #5040, #7975, #7607, #164, #12761, #4743, #2240, #5902, #13130, #9923, #7648, #5961, #13712, #10217, #4406, #13595, #5603, #4626, #13907, #6697, #3758, #3856, #9272, #7291, #228, #14428, #11130, #6896, #2568, #8438, #7243, #15413, #10296, #6167, #7164, #12743 ) ) ;
#13313 = CARTESIAN_POINT ( 'NONE',  ( 5.000000000000000000, -22.00000000000000000, 0.000000000000000000 ) ) ;
#13314 = DIRECTION ( 'NONE',  ( 0.000000000000000000, 1.000000000000000000, 0.000000000000000000 ) ) ;
#13315 = CARTESIAN_POINT ( 'NONE',  ( 19.99999999999956657, -8.786575603324269439E-13, -13.00000000000000000 ) ) ;
#13316 = CARTESIAN_POINT ( 'NONE',  ( 1.846868145590736310, -22.87500000136559564, 4.458734124999999437 ) ) ;
#13317 = CARTESIAN_POINT ( 'NONE',  ( 0.000000000000000000, 0.000000000000000000, -0.5776712190230133270 ) ) ;
#13318 = CIRCLE ( 'NONE', #1465, 29.99999999999999289 ) ;
#13319 = DIRECTION ( 'NONE',  ( -0.000000000000000000, -1.000000000000000000, -0.000000000000000000 ) ) ;
#13320 = CARTESIAN_POINT ( 'NONE',  ( -3.535533905932737309, -30.75000000273118772, -3.535533905932738197 ) ) ;
#13321 = DIRECTION ( 'NONE',  ( -0.000000000000000000, -0.000000000000000000, -1.000000000000000000 ) ) ;
#13322 = ADVANCED_FACE ( 'NONE', ( #6712 ), #7384, .F. ) ;
#13324 = EDGE_CURVE ( 'NONE', #7414, #635, #2005, .T. ) ;
#13323 = VERTEX_POINT ( 'NONE', #1766 ) ;
#13325 = PRODUCT_DEFINITION_FORMATION_WITH_SPECIFIED_SOURCE ( 'ANY', '', #9775, .NOT_KNOWN. ) ;
#13326 = EDGE_CURVE ( 'NONE', #7997, #1698, #10656, .T. ) ;
#13327 = EDGE_CURVE ( 'NONE', #12101, #15747, #13062, .T. ) ;
#13328 =( LENGTH_UNIT ( ) NAMED_UNIT ( * ) SI_UNIT ( .MILLI., .METRE. ) );
#13329 = VERTEX_POINT ( 'NONE', #11769 ) ;
#13330 = DIRECTION ( 'NONE',  ( 0.000000000000000000, -1.000000000000000000, 0.000000000000000000 ) ) ;
#13331 = VERTEX_POINT ( 'NONE', #15351 ) ;
#13332 = VECTOR ( 'NONE', #765, 1000.000000000000000 ) ;
#13333 = DIRECTION ( 'NONE',  ( 0.000000000000000000, 1.000000000000000000, -1.287488025362403787E-15 ) ) ;
#13334 = DIRECTION ( 'NONE',  ( 0.000000000000000000, 0.000000000000000000, -1.000000000000000000 ) ) ;
#13335 = AXIS2_PLACEMENT_3D ( 'NONE', #8193, #6978, #2344 ) ;
#13336 = CARTESIAN_POINT ( 'NONE',  ( 4.276409079477644148, 1.261996585732577891, 1.687500001365593194 ) ) ;
#13337 = CARTESIAN_POINT ( 'NONE',  ( 0.000000000000000000, -20.00000000000000000, 0.000000000000000000 ) ) ;
#13338 = CARTESIAN_POINT ( 'NONE',  ( 3.033343224707661712, -3.753672977998669946, -0.7499999986344074721 ) ) ;
#13339 =( LENGTH_UNIT ( ) NAMED_UNIT ( * ) SI_UNIT ( .MILLI., .METRE. ) );
#13340 = VECTOR ( 'NONE', #11697, 1000.000000000000000 ) ;
#13341 = CARTESIAN_POINT ( 'NONE',  ( -28.86751345948126257, 0.000000000000000000, -50.00000000000000711 ) ) ;
#13342 = ORIENTED_EDGE ( 'NONE', *, *, #9442, .T. ) ;
#13344 = AXIS2_PLACEMENT_3D ( 'NONE', #14491, #8526, #11096 ) ;
#13343 = CARTESIAN_POINT ( 'NONE',  ( 24.26932219902320043, 40.00000000000000000, 5.999999999999992895 ) ) ;
#13345 = ADVANCED_FACE ( 'NONE', ( #13145 ), #722, .T. ) ;
#13346 = SURFACE_STYLE_USAGE ( .BOTH. , #3491 ) ;
#13347 = ORIENTED_EDGE ( 'NONE', *, *, #7093, .F. ) ;
#13348 = CARTESIAN_POINT ( 'NONE',  ( -0.5711823568785977523, -5.381735091635034607, -1.312500000000000222 ) ) ;
#13349 = DIRECTION ( 'NONE',  ( -0.000000000000000000, -1.000000000000000000, -0.000000000000000000 ) ) ;
#13350 = VERTEX_POINT ( 'NONE', #2078 ) ;
#13351 = VECTOR ( 'NONE', #3415, 1000.000000000000000 ) ;
#13352 = ORIENTED_EDGE ( 'NONE', *, *, #7586, .T. ) ;
#13353 = CARTESIAN_POINT ( 'NONE',  ( -2.131511515620587272, -3.916244202832140253, -1.937499998634406584 ) ) ;
#13354 =( NAMED_UNIT ( * ) SI_UNIT ( $, .STERADIAN. ) SOLID_ANGLE_UNIT ( ) );
#13355 = EDGE_CURVE ( 'NONE', #11193, #7310, #9058, .T. ) ;
#13356 = CIRCLE ( 'NONE', #744, 3.499999999999999556 ) ;
#13357 = DIRECTION ( 'NONE',  ( 0.8660254037844387076, 0.000000000000000000, -0.4999999999999998335 ) ) ;
#13358 = FACE_OUTER_BOUND ( 'NONE', #4138, .T. ) ;
#13359 = AXIS2_PLACEMENT_3D ( 'NONE', #631, #3200, #3361 ) ;
#13360 = PLANE ( 'NONE',  #1253 ) ;
#13361 = VECTOR ( 'NONE', #12543, 1000.000000000000227 ) ;
#13362 = CARTESIAN_POINT ( 'NONE',  ( 2.390265326283148806, 4.391654775818395251, -1.749999997268814722 ) ) ;
#13363 = SURFACE_SIDE_STYLE ('',( #10949 ) ) ;
#13364 = CARTESIAN_POINT ( 'NONE',  ( -5.000000000000000888, -22.68750000273119127, -2.071067811865475949 ) ) ;
#13365 = CARTESIAN_POINT ( 'NONE',  ( 4.458734124999999437, -26.62500000136559564, -1.846868145590734978 ) ) ;
#13366 = CARTESIAN_POINT ( 'NONE',  ( -4.799145180956616130, 0.5093500532425063732, -2.874999998634407472 ) ) ;
#13367 = CARTESIAN_POINT ( 'NONE',  ( 0.000000000000000000, 0.000000000000000000, -8.499999999999996447 ) ) ;
#13368 = ORIENTED_EDGE ( 'NONE', *, *, #2813, .T. ) ;
#13369 = VECTOR ( 'NONE', #6808, 1000.000000000000000 ) ;
#13370 = VERTEX_POINT ( 'NONE', #877 ) ;
#13371 = AXIS2_PLACEMENT_3D ( 'NONE', #11381, #3705, #6305 ) ;
#13372 = ORIENTED_EDGE ( 'NONE', *, *, #12346, .T. ) ;
#13373 = PRODUCT_DEFINITION_SHAPE ( 'NONE', 'NONE',  #6723 ) ;
#13374 = CARTESIAN_POINT ( 'NONE',  ( 4.458734124999999437, -23.68750000136559564, 0.000000000000000000 ) ) ;
#13375 = CARTESIAN_POINT ( 'NONE',  ( -3.535533905932737309, -23.75000000273118772, -3.535533905932738197 ) ) ;
#13376 = CARTESIAN_POINT ( 'NONE',  ( 2.071067811865461294, -29.93750000273118062, -5.000000000000014211 ) ) ;
#13377 = ADVANCED_FACE ( 'NONE', ( #2460 ), #8398, .F. ) ;
#13378 = DIRECTION ( 'NONE',  ( -1.000000000000000000, 0.000000000000000000, -0.000000000000000000 ) ) ;
#13379 = FACE_OUTER_BOUND ( 'NONE', #8845, .T. ) ;
#13380 = EDGE_CURVE ( 'NONE', #7223, #715, #14846, .T. ) ;
#13381 = CARTESIAN_POINT ( 'NONE',  ( 3.535533905932736864, -22.12500000000000000, 3.535533905932738641 ) ) ;
#13382 = CARTESIAN_POINT ( 'NONE',  ( 4.391654775818395251, -2.390265326283149694, -1.125000000000000888 ) ) ;
#13383 = DIRECTION ( 'NONE',  ( -0.000000000000000000, 1.000000000000000000, -0.000000000000000000 ) ) ;
#13384 = CARTESIAN_POINT ( 'NONE',  ( -3.364693435263333310, -3.390744528670103453, -0.1614628718363220472 ) ) ;
#13385 = CARTESIAN_POINT ( 'NONE',  ( 1.846868145590735200, -25.25000000136559564, -4.458734125000000326 ) ) ;
#13386 = CARTESIAN_POINT ( 'NONE',  ( -1.261996585732579224, 4.276409079477648589, -2.312499998634407028 ) ) ;
#13387 = ORIENTED_EDGE ( 'NONE', *, *, #6750, .T. ) ;
#13388 = FACE_BOUND ( 'NONE', #642, .T. ) ;
#13389 = ORIENTED_EDGE ( 'NONE', *, *, #10395, .T. ) ;
#13390 = ORIENTED_EDGE ( 'NONE', *, *, #12927, .F. ) ;
#13391 = CARTESIAN_POINT ( 'NONE',  ( 25.00000000000000000, 0.000000000000000000, 2.055000000000000160 ) ) ;
#13392 = CARTESIAN_POINT ( 'NONE',  ( 3.152801135295366208, -26.56250000136559564, 3.152801135295367985 ) ) ;
#13393 = CARTESIAN_POINT ( 'NONE',  ( 12.67949192431126093, -37.00000000000000711, -61.96152422706632024 ) ) ;
#13394 = ORIENTED_EDGE ( 'NONE', *, *, #10013, .F. ) ;
#13395 = CARTESIAN_POINT ( 'NONE',  ( -9.184850993605147944E-16, -28.25000000000000000, 5.000000000000000000 ) ) ;
#13396 = FACE_OUTER_BOUND ( 'NONE', #2743, .T. ) ;
#13397 = EDGE_CURVE ( 'NONE', #8315, #12412, #10692, .T. ) ;
#13398 = CARTESIAN_POINT ( 'NONE',  ( 3.999999999999999112, 2.309401076758497595, -3.504271511726784194 ) ) ;
#13399 = CARTESIAN_POINT ( 'NONE',  ( -6.762176242291807225E-13, 37.00000000000000000, 70.14999999999929514 ) ) ;
#13400 = ADVANCED_FACE ( 'NONE', ( #2229 ), #4978, .F. ) ;
#13401 = CARTESIAN_POINT ( 'NONE',  ( 3.152801135295366208, -22.81250000136559564, 3.152801135295367985 ) ) ;
#13402 = FACE_BOUND ( 'NONE', #8802, .T. ) ;
#13403 = CARTESIAN_POINT ( 'NONE',  ( 3.061616997868383141E-16, -31.75000000000000000, -5.000000000000000000 ) ) ;
#13404 = LINE ( 'NONE', #9784, #11173 ) ;
#13405 = CARTESIAN_POINT ( 'NONE',  ( -36.99999999999999289, -11.00000000000000178, 2.000000000000830891 ) ) ;
#13406 = CARTESIAN_POINT ( 'NONE',  ( 2.143131898507869826E-15, 40.00000000000000000, -67.50000000000000000 ) ) ;
#13407 = ORIENTED_EDGE ( 'NONE', *, *, #2916, .F. ) ;
#13408 = ORIENTED_EDGE ( 'NONE', *, *, #10966, .F. ) ;
#13409 = CARTESIAN_POINT ( 'NONE',  ( 2.344047193898588954, 3.265465875126468021, -5.031375706690542042E-16 ) ) ;
#13410 = EDGE_LOOP ( 'NONE', ( #10524, #6239, #14702 ) ) ;
#13411 = CARTESIAN_POINT ( 'NONE',  ( 16.49999999999956657, -8.782289339527253835E-13, -13.00000000000000000 ) ) ;
#13412 = ADVANCED_FACE ( 'NONE', ( #7185, #3608, #1263, #14601, #14522, #3442 ), #15903, .F. ) ;
#13413 = PRODUCT_DEFINITION ( 'UNKNOWN', '', #9989, #4148 ) ;
#13414 = EDGE_CURVE ( 'NONE', #1037, #10616, #3472, .T. ) ;
#13415 = DIRECTION ( 'NONE',  ( 0.000000000000000000, 1.000000000000000000, 0.000000000000000000 ) ) ;
#13416 = CARTESIAN_POINT ( 'NONE',  ( -1.261996585732579224, 4.276409079477648589, 0.9375000013655925279 ) ) ;
#13417 = CARTESIAN_POINT ( 'NONE',  ( 0.000000000000000000, -20.00000000000000000, 0.000000000000000000 ) ) ;
#13418 = CARTESIAN_POINT ( 'NONE',  ( -3.916244202832140253, 2.131511515620587272, -3.187499998634407916 ) ) ;
#13419 = DIRECTION ( 'NONE',  ( -0.000000000000000000, -0.000000000000000000, 1.000000000000000000 ) ) ;
#13420 = DIRECTION ( 'NONE',  ( 0.000000000000000000, 0.000000000000000000, 1.000000000000000000 ) ) ;
#13421 = ORIENTED_EDGE ( 'NONE', *, *, #8220, .T. ) ;
#13422 = CARTESIAN_POINT ( 'NONE',  ( 4.000000000000000000, -2.511475576507276042, -3.469253905236643565 ) ) ;
#13423 = FACE_OUTER_BOUND ( 'NONE', #2596, .T. ) ;
#13424 = ORIENTED_EDGE ( 'NONE', *, *, #641, .T. ) ;
#13425 = CARTESIAN_POINT ( 'NONE',  ( -3.753672977998669502, -3.033343224707661712, -2.999999998634409248 ) ) ;
#13426 = CARTESIAN_POINT ( 'NONE',  ( 0.000000000000000000, -13.00000000000000178, 5.000000000000000000 ) ) ;
#13427 = EDGE_CURVE ( 'NONE', #15871, #4627, #5021, .T. ) ;
#13428 = CARTESIAN_POINT ( 'NONE',  ( -114.9999999999999716, -10.00000000000000888, -17.50000000000000000 ) ) ;
#13429 = PLANE ( 'NONE',  #10265 ) ;
#13430 = LINE ( 'NONE', #9889, #81 ) ;
#13431 = LINE ( 'NONE', #5778, #15213 ) ;
#13432 = CARTESIAN_POINT ( 'NONE',  ( -3.401574460001764777, 4.209348295687701302, -1.562499997268814056 ) ) ;
#13433 = DIRECTION ( 'NONE',  ( 0.000000000000000000, 0.000000000000000000, 1.000000000000000000 ) ) ;
#13434 = CARTESIAN_POINT ( 'NONE',  ( -1.846868145590737420, -26.00000000136560274, 4.458734124999997661 ) ) ;
#13435 = CARTESIAN_POINT ( 'NONE',  ( -4.458734125000000326, -21.87500000136559208, 1.846868145590734089 ) ) ;
#13436 = CARTESIAN_POINT ( 'NONE',  ( -3.916244202832140253, 2.131511515620587272, -5.937499998634407028 ) ) ;
#13437 = CARTESIAN_POINT ( 'NONE',  ( -6.762176242291807225E-13, 50.00000000000000000, 64.84999999999932641 ) ) ;
#13438 = ORIENTED_EDGE ( 'NONE', *, *, #10490, .T. ) ;
#13439 = ORIENTED_EDGE ( 'NONE', *, *, #10875, .F. ) ;
#13440 =( NAMED_UNIT ( * ) SI_UNIT ( $, .STERADIAN. ) SOLID_ANGLE_UNIT ( ) );
#13441 = ORIENTED_EDGE ( 'NONE', *, *, #2301, .F. ) ;
#13442 = CARTESIAN_POINT ( 'NONE',  ( -3.152801135295367985, -22.06250000136559564, 3.152801135295367096 ) ) ;
#13443 = LINE ( 'NONE', #10730, #171 ) ;
#13444 = CYLINDRICAL_SURFACE ( 'NONE', #6578, 5.000000000000000888 ) ;
#13445 = DIRECTION ( 'NONE',  ( 1.000000000000000000, -0.000000000000000000, -1.239088197126290570E-16 ) ) ;
#13446 = CARTESIAN_POINT ( 'NONE',  ( -44.99999999999999289, -11.00000000000000178, -3.999999999999170885 ) ) ;
#13447 =( BOUNDED_CURVE ( )  B_SPLINE_CURVE ( 2, ( #124, #8692, #13680, #1243, #5046, #6346, #11180, #8935, #14995 ),
 .UNSPECIFIED., .F., .F. ) 
 B_SPLINE_CURVE_WITH_KNOTS ( ( 3, 2, 2, 2, 3 ),
 ( 0.3750000000000000000, 0.3875000000000000111, 0.4000000000000000222, 0.4125000000000000333, 0.4250000000000000444 ),
 .UNSPECIFIED. ) 
 CURVE ( )  GEOMETRIC_REPRESENTATION_ITEM ( )  RATIONAL_B_SPLINE_CURVE ( ( 1.000000000000000000, 0.9238795325112867385, 1.000000000000000000, 0.9238795325112867385, 1.000000000000000000, 0.9238795325112867385, 1.000000000000000000, 0.9238795325112864054, 1.000000000000000444 ) ) 
 REPRESENTATION_ITEM ( '' )  );
#13448 = CARTESIAN_POINT ( 'NONE',  ( -5.000000000000000888, -22.43749999999999645, 2.071067811865474617 ) ) ;
#13449 = CARTESIAN_POINT ( 'NONE',  ( -4.795541693661363958, -1.415196051561583790, -0.5000000000000004441 ) ) ;
#13450 = CARTESIAN_POINT ( 'NONE',  ( -2.071067811865482167, -27.68750000000000000, -4.999999999999992895 ) ) ;
#13451 = CARTESIAN_POINT ( 'NONE',  ( -8.190561711645485556E-16, -27.68750000136559564, 4.458734124999999437 ) ) ;
#13452 = CARTESIAN_POINT ( 'NONE',  ( 4.799145180956616130, -0.5093500532425063732, -2.624999998634407028 ) ) ;
#13453 = ORIENTED_EDGE ( 'NONE', *, *, #14547, .F. ) ;
#13454 = FACE_OUTER_BOUND ( 'NONE', #3513, .T. ) ;
#13455 = VERTEX_POINT ( 'NONE', #2154 ) ;
#13456 = EDGE_LOOP ( 'NONE', ( #8021, #5641, #9477, #15371 ) ) ;
#13457 = DIRECTION ( 'NONE',  ( 0.000000000000000000, 0.000000000000000000, 1.000000000000000000 ) ) ;
#13458 = CARTESIAN_POINT ( 'NONE',  ( 4.458734124999999437, -26.50000000136559208, 1.846868145590737864 ) ) ;
#13459 = EDGE_CURVE ( 'NONE', #6007, #3972, #14061, .T. ) ;
#13460 = DIRECTION ( 'NONE',  ( -1.000000000000000000, 0.000000000000000000, -3.343241100358131282E-16 ) ) ;
#13461 = VERTEX_POINT ( 'NONE', #12004 ) ;
#13462 = CIRCLE ( 'NONE', #12178, 9.999999999999994671 ) ;
#13463 = PLANE ( 'NONE',  #8428 ) ;
#13464 = AXIS2_PLACEMENT_3D ( 'NONE', #1030, #4828, #10815 ) ;
#13465 = CYLINDRICAL_SURFACE ( 'NONE', #2806, 5.000000000000000000 ) ;
#13466 = LINE ( 'NONE', #11076, #12849 ) ;
#13467 = CARTESIAN_POINT ( 'NONE',  ( -115.0000000000000142, -25.00000000000001066, -17.50000000000000000 ) ) ;
#13468 = CARTESIAN_POINT ( 'NONE',  ( -4.458734125000000326, -22.25000000136559564, -1.846868145590735644 ) ) ;
#13469 = DIRECTION ( 'NONE',  ( -0.000000000000000000, 0.000000000000000000, 1.000000000000000000 ) ) ;
#13470 = LINE ( 'NONE', #4856, #12089 ) ;
#13471 = CARTESIAN_POINT ( 'NONE',  ( -9.184850993605147944E-16, -30.37500000273118772, 5.000000000000000000 ) ) ;
#13472 = DIRECTION ( 'NONE',  ( 0.000000000000000000, -1.000000000000000000, 1.287488025362403787E-15 ) ) ;
#13473 = AXIS2_PLACEMENT_3D ( 'NONE', #15492, #4646, #3193 ) ;
#13474 = CARTESIAN_POINT ( 'NONE',  ( 4.458734124999999437, -30.43750000136559564, 0.000000000000000000 ) ) ;
#13475 = DIRECTION ( 'NONE',  ( -0.000000000000000000, -1.000000000000000000, -0.000000000000000000 ) ) ;
#13476 = VERTEX_POINT ( 'NONE', #5879 ) ;
#13477 =( LENGTH_UNIT ( ) NAMED_UNIT ( * ) SI_UNIT ( .MILLI., .METRE. ) );
#13479 = EDGE_LOOP ( 'NONE', ( #9941, #4818, #11210, #41 ) ) ;
#13478 = ADVANCED_FACE ( 'NONE', ( #10814 ), #13444, .F. ) ;
#13480 = CARTESIAN_POINT ( 'NONE',  ( 4.000000000000000000, 2.309401076758515803, -0.4999999999999995559 ) ) ;
#13481 = ADVANCED_FACE ( 'NONE', ( #1028, #5962 ), #12238, .F. ) ;
#13482 = ORIENTED_EDGE ( 'NONE', *, *, #11068, .F. ) ;
#13483 = DIRECTION ( 'NONE',  ( -0.000000000000000000, -1.000000000000000000, -0.000000000000000000 ) ) ;
#13484 = CARTESIAN_POINT ( 'NONE',  ( 23.49999999999956657, -8.782289339527253835E-13, 1.500000000000000000 ) ) ;
#13485 = CARTESIAN_POINT ( 'NONE',  ( 0.5093500532425063732, 4.799145180956616130, -3.124999998634407916 ) ) ;
#13486 = APPLICATION_PROTOCOL_DEFINITION ( 'draft international standard', 'automotive_design', 1998, #2780 ) ;
#13487 = CARTESIAN_POINT ( 'NONE',  ( -1.261996585732579224, 4.276409079477648589, -2.312499998634407028 ) ) ;
#13488 = FACE_OUTER_BOUND ( 'NONE', #12578, .T. ) ;
#13489 = CARTESIAN_POINT ( 'NONE',  ( 35.00000000000000000, 40.00000000000000000, -2.650000000000001243 ) ) ;
#13490 = CARTESIAN_POINT ( 'NONE',  ( -9.184850993605147944E-16, -22.25000000000000000, 5.000000000000000000 ) ) ;
#13491 =( REPRESENTATION_RELATIONSHIP ('NONE','NONE', #4176, #4696 ) REPRESENTATION_RELATIONSHIP_WITH_TRANSFORMATION ( #6816 )SHAPE_REPRESENTATION_RELATIONSHIP( ) );
#13492 = FILL_AREA_STYLE ('',( #7306 ) ) ;
#13493 = EDGE_CURVE ( 'NONE', #10237, #6755, #3653, .T. ) ;
#13494 = EDGE_LOOP ( 'NONE', ( #5619, #1387, #5478, #5342 ) ) ;
#13495 = LINE ( 'NONE', #9881, #4388 ) ;
#13496 = EDGE_LOOP ( 'NONE', ( #15730, #10372, #15139, #11507, #5270 ) ) ;
#13497 = EDGE_CURVE ( 'NONE', #6259, #6791, #1584, .T. ) ;
#13498 =( GEOMETRIC_REPRESENTATION_CONTEXT ( 3 ) GLOBAL_UNCERTAINTY_ASSIGNED_CONTEXT ( ( #1722 ) ) GLOBAL_UNIT_ASSIGNED_CONTEXT ( ( #14214, #11235, #5562 ) ) REPRESENTATION_CONTEXT ( 'NONE', 'WORKASPACE' ) );
#13499 = VERTEX_POINT ( 'NONE', #5303 ) ;
#13500 = CARTESIAN_POINT ( 'NONE',  ( 0.5093500532425063732, 4.799145180956616130, -4.374999998634405252 ) ) ;
#13501 = AXIS2_PLACEMENT_3D ( 'NONE', #1772, #6719, #261 ) ;
#13502 = DIRECTION ( 'NONE',  ( -1.000000000000000000, -0.000000000000000000, -0.000000000000000000 ) ) ;
#13503 = CARTESIAN_POINT ( 'NONE',  ( -3.680118525130244400, 2.494084732383327285, -0.3507732604232449702 ) ) ;
#13504 = CARTESIAN_POINT ( 'NONE',  ( -35.00000000000000000, 40.00000000000000000, 0.000000000000000000 ) ) ;
#13505 = LINE ( 'NONE', #2442, #8350 ) ;
#13506 = CARTESIAN_POINT ( 'NONE',  ( -3.535533905932737309, -30.75000000273118772, -3.535533905932738197 ) ) ;
#13507 = AXIS2_PLACEMENT_3D ( 'NONE', #1413, #12233, #13520 ) ;
#13508 = CARTESIAN_POINT ( 'NONE',  ( -4.209348295687703967, -3.401574460001763001, 0.6875000027311841677 ) ) ;
#13509 =( LENGTH_UNIT ( ) NAMED_UNIT ( * ) SI_UNIT ( .MILLI., .METRE. ) );
#13510 = CARTESIAN_POINT ( 'NONE',  ( -2.071067811865478170, -22.43750000273118772, 5.000000000000000000 ) ) ;
#13511 = CARTESIAN_POINT ( 'NONE',  ( 4.458734124999999437, -27.68750000136559564, 0.000000000000000000 ) ) ;
#13512 = AXIS2_PLACEMENT_3D ( 'NONE', #9750, #14688, #12322 ) ;
#13513 = CARTESIAN_POINT ( 'NONE',  ( 0.000000000000000000, -20.00000000000000000, 0.000000000000000000 ) ) ;
#13514 = CARTESIAN_POINT ( 'NONE',  ( -4.799145180956616130, 0.5093500532425063732, -5.874999998634406140 ) ) ;
#13515 = PLANE ( 'NONE',  #14348 ) ;
#13516 = EDGE_CURVE ( 'NONE', #9104, #482, #10455, .T. ) ;
#13517 = ORIENTED_EDGE ( 'NONE', *, *, #9786, .T. ) ;
#13518 = EDGE_LOOP ( 'NONE', ( #9717, #9128, #5075, #872 ) ) ;
#13519 = EDGE_CURVE ( 'NONE', #11302, #6, #387, .T. ) ;
#13520 = DIRECTION ( 'NONE',  ( 1.000000000000000000, 0.000000000000000000, 0.000000000000000000 ) ) ;
#13521 = VERTEX_POINT ( 'NONE', #15009 ) ;
#13522 = CARTESIAN_POINT ( 'NONE',  ( 4.458734124999999437, -22.75000000136559208, 1.846868145590737864 ) ) ;
#13523 = CARTESIAN_POINT ( 'NONE',  ( 2.467663300281918521E-15, 40.00000000000000000, -70.14999999999999147 ) ) ;
#13524 = MECHANICAL_DESIGN_GEOMETRIC_PRESENTATION_REPRESENTATION (  '', ( #398 ), #410 ) ;
#13525 = CARTESIAN_POINT ( 'NONE',  ( -5.000000000000000000, -27.62500000273118772, -6.123233995736766282E-16 ) ) ;
#13526 = AXIS2_PLACEMENT_3D ( 'NONE', #15861, #2113, #8359 ) ;
#13527 = DIRECTION ( 'NONE',  ( -0.000000000000000000, -1.000000000000000000, -0.000000000000000000 ) ) ;
#13528 = LINE ( 'NONE', #13446, #3931 ) ;
#13529 = CARTESIAN_POINT ( 'NONE',  ( -115.2406606923553056, -116.0588903632565092, 17.50000000000000711 ) ) ;
#13530 = CARTESIAN_POINT ( 'NONE',  ( 4.391654775818395251, -2.390265326283149694, -2.125000000000001776 ) ) ;
#13531 = FACE_OUTER_BOUND ( 'NONE', #12788, .T. ) ;
#13532 = DIRECTION ( 'NONE',  ( 0.4999999999999998335, 0.000000000000000000, 0.8660254037844387076 ) ) ;
#13533 = CARTESIAN_POINT ( 'NONE',  ( 3.152801135295367541, -28.31250000136559564, -3.152801135295367541 ) ) ;
#13534 = CARTESIAN_POINT ( 'NONE',  ( 3.753672977998667726, 3.033343224707664376, -2.499999998634408804 ) ) ;
#13535 = ORIENTED_EDGE ( 'NONE', *, *, #5736, .T. ) ;
#13536 = AXIS2_PLACEMENT_3D ( 'NONE', #7699, #5098, #9940 ) ;
#13537 = DIRECTION ( 'NONE',  ( -0.8660254037844408170, -0.000000000000000000, -0.4999999999999961142 ) ) ;
#13538 = EDGE_LOOP ( 'NONE', ( #5099, #8134, #8551, #14211 ) ) ;
#13539 = VERTEX_POINT ( 'NONE', #3925 ) ;
#13541 = DIRECTION ( 'NONE',  ( -0.000000000000000000, 1.000000000000000000, -0.000000000000000000 ) ) ;
#13540 = AXIS2_PLACEMENT_3D ( 'NONE', #6320, #2908, #10285 ) ;
#13542 = EDGE_CURVE ( 'NONE', #14017, #7703, #12478, .T. ) ;
#13543 = CARTESIAN_POINT ( 'NONE',  ( -4.458734124999999437, -22.93750000136559564, -5.460374474430324690E-16 ) ) ;
#13544 = DIRECTION ( 'NONE',  ( -1.000000000000000000, -0.000000000000000000, -0.000000000000000000 ) ) ;
#13545 = VERTEX_POINT ( 'NONE', #12402 ) ;
#13546 = CYLINDRICAL_SURFACE ( 'NONE', #12003, 2.649999999999992806 ) ;
#13547 =( BOUNDED_SURFACE ( )  B_SPLINE_SURFACE ( 1, 2, ( 
 ( #8280, #13170, #2106, #15779, #7050, #983, #13320, #1053, #3552, #5987, #11954, #5915, #13471, #6394, #12430, #6155, #7362, #7608, #7451, #12270, #10029, #9783, #14717, #12593, #2409, #5007, #13803, #3954, #4857, #13557, #11230, #9859, #14875, #8822, #12507, #5178, #6313, #11082, #2490, #1211, #11313, #1366, #15, #4933, #1449, #12357, #14791, #14964, #3638, #6066, #1289, #3711, #8898, #8583, #8658, #2739, #15039, #11150, #175, #10996, #15935, #263, #5094, #10107, #7696, #6234, #90, #2656, #9936, #3798, #8742, #13648, #2577, #7528, #3880, #13723, #10425, #13895, #2900, #10354, #15360, #12669, #12748, #5577, #15448, #12831, #1693, #7850, #5495, #4280, #14225, #3073, #6634, #11548, #1609, #9142, #14144, #9221, #1774, #4369, #11465, #500, #3149, #9066, #10514, #6722, #413, #5422, #10188, #11387, #8016, #8094, #12913, #10276, #1537, #11624, #15111, #1847, #6790, #11698, #6475, #9303, #14053, #2980, #653, #15281, #339, #574, #4195, #5252, #5337, #15204, #4032, #8983, #7934, #2824, #7778, #6550, #4118, #13968, #963, #7110, #2161, #10599, #9531, #1035, #15598, #3309, #10663, #12095, #10822, #6873, #11780, #2011, #10891, #14460, #3381, #13223, #15523, #733, #13297 ),
 ( #8261, #3531, #4673, #5889, #15762, #13153, #12014, #9597, #5658, #15832, #4515, #2088, #3452, #5805, #7195, #13073, #7033, #9376, #9672, #14534, #8405, #4752, #6960, #11933, #14610, #9450, #5970, #8332, #11861, #885, #4439, #14299, #2241, #12988, #1924, #5728, #3222, #8171, #808, #14381, #10742, #15679, #4593, #11292, #4988, #70, #13704, #8638, #8487, #3774, #13533, #13626, #7341, #12246, #7589, #7267, #12333, #4834, #10971, #14697, #13451, #9759, #12410, #2556, #7509, #6046, #9913, #12487, #11059, #14770, #6132, #1427, #1106, #15018, #15913, #7428, #243, #6374, #12168, #1468, #1346, #1187, #1270, #11208, #14942, #5161, #8720, #8563, #4913, #3618, #8800, #14853, #2392, #9838, #10003, #3692, #2468, #6293, #6215, #13385, #11131, #152, #10091, #5072, #3861, #2323, #2637, #9046, #14030, #10489, #8877, #7908, #2957, #9121, #1520, #476, #7994, #6531, #10253, #1592, #3047, #12572, #3933, #11370, #2880, #11680, #1827, #2716, #11445, #12808, #7761, #12728, #6701, #10405, #12895, #4174, #4010, #391, #321, #4256, #10336, #8961, #5231, #5476, #5311, #10167, #1751, #7674, #13783, #15179, #15090, #6772, #6457, #2805, #633, #5554, #13949, #11605, #13872, #12652, #9201 ) ),
 .UNSPECIFIED., .F., .F., .F. ) 
 B_SPLINE_SURFACE_WITH_KNOTS ( ( 2, 2 ),
 ( 3, 2, 2, 2, 2, 2, 2, 2, 2, 2, 2, 2, 2, 2, 2, 2, 2, 2, 2, 2, 2, 2, 2, 2, 2, 2, 2, 2, 2, 2, 2, 2, 2, 2, 2, 2, 2, 2, 2, 2, 2, 2, 2, 2, 2, 2, 2, 2, 2, 2, 2, 2, 2, 2, 2, 2, 2, 2, 2, 2, 2, 2, 2, 2, 2, 2, 2, 2, 2, 2, 2, 2, 2, 2, 2, 2, 2, 2, 2, 2, 3 ),
 ( 0.000000000000000000, 1.000000000000000000 ),
 ( 0.000000000000000000, 0.01250000000000000069, 0.02500000000000000139, 0.03749999999999999861, 0.05000000000000000278, 0.06250000000000000000, 0.07499999999999999722, 0.08749999999999999445, 0.1000000000000000056, 0.1125000000000000028, 0.1250000000000000000, 0.1375000000000000111, 0.1499999999999999944, 0.1625000000000000056, 0.1749999999999999889, 0.1875000000000000000, 0.2000000000000000111, 0.2124999999999999944, 0.2250000000000000056, 0.2374999999999999889, 0.2500000000000000000, 0.2625000000000000111, 0.2750000000000000222, 0.2874999999999999778, 0.2999999999999999889, 0.3125000000000000000, 0.3250000000000000111, 0.3375000000000000222, 0.3499999999999999778, 0.3624999999999999889, 0.3750000000000000000, 0.3875000000000000111, 0.4000000000000000222, 0.4124999999999999778, 0.4249999999999999889, 0.4375000000000000000, 0.4500000000000000111, 0.4625000000000000222, 0.4749999999999999778, 0.4874999999999999889, 0.5000000000000000000, 0.5124999999999999556, 0.5250000000000000222, 0.5374999999999999778, 0.5500000000000000444, 0.5625000000000000000, 0.5749999999999999556, 0.5875000000000000222, 0.5999999999999999778, 0.6125000000000000444, 0.6250000000000000000, 0.6374999999999999556, 0.6500000000000000222, 0.6624999999999999778, 0.6750000000000000444, 0.6875000000000000000, 0.6999999999999999556, 0.7125000000000000222, 0.7249999999999999778, 0.7375000000000000444, 0.7500000000000000000, 0.7624999999999999556, 0.7750000000000000222, 0.7874999999999999778, 0.8000000000000000444, 0.8125000000000000000, 0.8249999999999999556, 0.8375000000000000222, 0.8499999999999999778, 0.8625000000000000444, 0.8750000000000000000, 0.8874999999999999556, 0.9000000000000000222, 0.9124999999999999778, 0.9250000000000000444, 0.9375000000000000000, 0.9499999999999999556, 0.9625000000000000222, 0.9749999999999999778, 0.9875000000000000444, 1.000000000000000000 ),
 .UNSPECIFIED. ) 
 GEOMETRIC_REPRESENTATION_ITEM ( )  RATIONAL_B_SPLINE_SURFACE ( (
 ( 1.000000000000000000, 0.9238795325112867385, 1.000000000000000000, 0.9238795325112867385, 1.000000000000000000, 0.9238795325112867385, 1.000000000000000000, 0.9238795325112867385, 1.000000000000000000, 0.9238795325112867385, 1.000000000000000000, 0.9238795325112867385, 1.000000000000000000, 0.9238795325112867385, 1.000000000000000000, 0.9238795325112867385, 1.000000000000000000, 0.9238795325112867385, 1.000000000000000000, 0.9238795325112867385, 1.000000000000000000, 0.9238795325112867385, 1.000000000000000000, 0.9238795325112867385, 1.000000000000000000, 0.9238795325112867385, 1.000000000000000000, 0.9238795325112867385, 1.000000000000000000, 0.9238795325112867385, 1.000000000000000000, 0.9238795325112867385, 1.000000000000000000, 0.9238795325112867385, 1.000000000000000000, 0.9238795325112867385, 1.000000000000000000, 0.9238795325112867385, 1.000000000000000000, 0.9238795325112867385, 1.000000000000000000, 0.9238795325112867385, 1.000000000000000000, 0.9238795325112867385, 1.000000000000000000, 0.9238795325112867385, 1.000000000000000000, 0.9238795325112867385, 1.000000000000000000, 0.9238795325112867385, 1.000000000000000000, 0.9238795325112867385, 1.000000000000000000, 0.9238795325112867385, 1.000000000000000000, 0.9238795325112867385, 1.000000000000000000, 0.9238795325112867385, 1.000000000000000000, 0.9238795325112867385, 1.000000000000000000, 0.9238795325112867385, 1.000000000000000000, 0.9238795325112867385, 1.000000000000000000, 0.9238795325112867385, 1.000000000000000000, 0.9238795325112867385, 1.000000000000000000, 0.9238795325112867385, 1.000000000000000000, 0.9238795325112867385, 1.000000000000000000, 0.9238795325112867385, 1.000000000000000000, 0.9238795325112867385, 1.000000000000000000, 0.9238795325112867385, 1.000000000000000000, 0.9238795325112867385, 1.000000000000000000, 0.9238795325112867385, 1.000000000000000000, 0.9238795325112867385, 1.000000000000000000, 0.9238795325112867385, 1.000000000000000000, 0.9238795325112867385, 1.000000000000000000, 0.9238795325112867385, 1.000000000000000000, 0.9238795325112867385, 1.000000000000000000, 0.9238795325112867385, 1.000000000000000000, 0.9238795325112867385, 1.000000000000000000, 0.9238795325112867385, 1.000000000000000000, 0.9238795325112867385, 1.000000000000000000, 0.9238795325112867385, 1.000000000000000000, 0.9238795325112867385, 1.000000000000000000, 0.9238795325112867385, 1.000000000000000000, 0.9238795325112867385, 1.000000000000000000, 0.9238795325112867385, 1.000000000000000000, 0.9238795325112867385, 1.000000000000000000, 0.9238795325112867385, 1.000000000000000000, 0.9238795325112867385, 1.000000000000000000, 0.9238795325112867385, 1.000000000000000000, 0.9238795325112867385, 1.000000000000000000, 0.9238795325112867385, 1.000000000000000000, 0.9238795325112867385, 1.000000000000000000, 0.9238795325112867385, 1.000000000000000000, 0.9238795325112867385, 1.000000000000000000, 0.9238795325112867385, 1.000000000000000000, 0.9238795325112867385, 1.000000000000000000, 0.9238795325112867385, 1.000000000000000000, 0.9238795325112867385, 1.000000000000000000, 0.9238795325112867385, 1.000000000000000000, 0.9238795325112867385, 1.000000000000000000, 0.9238795325112867385, 1.000000000000000000, 0.9238795325112867385, 1.000000000000000000, 0.9238795325112867385, 1.000000000000000000, 0.9238795325112867385, 1.000000000000000000, 0.9238795325112867385, 1.000000000000000000, 0.9238795325112867385, 1.000000000000000000, 0.9238795325112867385, 1.000000000000000000, 0.9238795325112867385, 1.000000000000000000, 0.9238795325112867385, 1.000000000000000000, 0.9238795325112867385, 1.000000000000000000),
 ( 1.000000000000000000, 0.9238795325112867385, 1.000000000000000000, 0.9238795325112867385, 1.000000000000000000, 0.9238795325112867385, 1.000000000000000000, 0.9238795325112867385, 1.000000000000000000, 0.9238795325112867385, 1.000000000000000000, 0.9238795325112867385, 1.000000000000000000, 0.9238795325112867385, 1.000000000000000000, 0.9238795325112867385, 1.000000000000000000, 0.9238795325112867385, 1.000000000000000000, 0.9238795325112867385, 1.000000000000000000, 0.9238795325112867385, 1.000000000000000000, 0.9238795325112867385, 1.000000000000000000, 0.9238795325112867385, 1.000000000000000000, 0.9238795325112867385, 1.000000000000000000, 0.9238795325112867385, 1.000000000000000000, 0.9238795325112867385, 1.000000000000000000, 0.9238795325112867385, 1.000000000000000000, 0.9238795325112867385, 1.000000000000000000, 0.9238795325112867385, 1.000000000000000000, 0.9238795325112867385, 1.000000000000000000, 0.9238795325112867385, 1.000000000000000000, 0.9238795325112867385, 1.000000000000000000, 0.9238795325112867385, 1.000000000000000000, 0.9238795325112867385, 1.000000000000000000, 0.9238795325112867385, 1.000000000000000000, 0.9238795325112867385, 1.000000000000000000, 0.9238795325112867385, 1.000000000000000000, 0.9238795325112867385, 1.000000000000000000, 0.9238795325112867385, 1.000000000000000000, 0.9238795325112867385, 1.000000000000000000, 0.9238795325112867385, 1.000000000000000000, 0.9238795325112867385, 1.000000000000000000, 0.9238795325112867385, 1.000000000000000000, 0.9238795325112867385, 1.000000000000000000, 0.9238795325112867385, 1.000000000000000000, 0.9238795325112867385, 1.000000000000000000, 0.9238795325112867385, 1.000000000000000000, 0.9238795325112867385, 1.000000000000000000, 0.9238795325112867385, 1.000000000000000000, 0.9238795325112867385, 1.000000000000000000, 0.9238795325112867385, 1.000000000000000000, 0.9238795325112867385, 1.000000000000000000, 0.9238795325112867385, 1.000000000000000000, 0.9238795325112867385, 1.000000000000000000, 0.9238795325112867385, 1.000000000000000000, 0.9238795325112867385, 1.000000000000000000, 0.9238795325112867385, 1.000000000000000000, 0.9238795325112867385, 1.000000000000000000, 0.9238795325112867385, 1.000000000000000000, 0.9238795325112867385, 1.000000000000000000, 0.9238795325112867385, 1.000000000000000000, 0.9238795325112867385, 1.000000000000000000, 0.9238795325112867385, 1.000000000000000000, 0.9238795325112867385, 1.000000000000000000, 0.9238795325112867385, 1.000000000000000000, 0.9238795325112867385, 1.000000000000000000, 0.9238795325112867385, 1.000000000000000000, 0.9238795325112867385, 1.000000000000000000, 0.9238795325112867385, 1.000000000000000000, 0.9238795325112867385, 1.000000000000000000, 0.9238795325112867385, 1.000000000000000000, 0.9238795325112867385, 1.000000000000000000, 0.9238795325112867385, 1.000000000000000000, 0.9238795325112867385, 1.000000000000000000, 0.9238795325112867385, 1.000000000000000000, 0.9238795325112867385, 1.000000000000000000, 0.9238795325112867385, 1.000000000000000000, 0.9238795325112867385, 1.000000000000000000, 0.9238795325112867385, 1.000000000000000000, 0.9238795325112867385, 1.000000000000000000, 0.9238795325112867385, 1.000000000000000000, 0.9238795325112867385, 1.000000000000000000, 0.9238795325112867385, 1.000000000000000000, 0.9238795325112867385, 1.000000000000000000, 0.9238795325112867385, 1.000000000000000000, 0.9238795325112867385, 1.000000000000000000, 0.9238795325112867385, 1.000000000000000000, 0.9238795325112867385, 1.000000000000000000, 0.9238795325112867385, 1.000000000000000000, 0.9238795325112867385, 1.000000000000000000) ) ) 
 REPRESENTATION_ITEM ( '' )  SURFACE ( )  );
#13548 = VECTOR ( 'NONE', #324, 1000.000000000000000 ) ;
#13549 = CARTESIAN_POINT ( 'NONE',  ( -67.50000000000000000, 37.00000000000000000, -2.650000000000699352 ) ) ;
#13550 = EDGE_CURVE ( 'NONE', #11846, #9639, #13614, .T. ) ;
#13551 = DIRECTION ( 'NONE',  ( -1.000000000000000000, 0.000000000000000000, 0.000000000000000000 ) ) ;
#13552 = DIRECTION ( 'NONE',  ( -0.000000000000000000, -1.000000000000000000, -0.000000000000000000 ) ) ;
#13553 = CARTESIAN_POINT ( 'NONE',  ( -4.458734124999999437, -25.18750000136559564, -5.460374474430324690E-16 ) ) ;
#13554 = CARTESIAN_POINT ( 'NONE',  ( -114.9999999999999716, -10.00000000000001243, -7.500000000000000000 ) ) ;
#13555 = ADVANCED_FACE ( 'NONE', ( #1657 ), #5389, .T. ) ;
#13556 = CARTESIAN_POINT ( 'NONE',  ( 2.000000000000000444, 3.464101615137754830, -3.142992957459231018 ) ) ;
#13557 = CARTESIAN_POINT ( 'NONE',  ( 2.071067811865476394, -29.31250000273118417, 5.000000000000000000 ) ) ;
#13558 = CARTESIAN_POINT ( 'NONE',  ( 2.131511515620586383, 3.916244202832140253, -8.437499998634409692 ) ) ;
#13559 = CARTESIAN_POINT ( 'NONE',  ( -3.152801135295367096, -31.06250000136559564, -3.152801135295367541 ) ) ;
#13560 = ORIENTED_EDGE ( 'NONE', *, *, #5447, .T. ) ;
#13561 = PRESENTATION_LAYER_ASSIGNMENT (  '', '', ( #7882 ) ) ;
#13562 =( NAMED_UNIT ( * ) PLANE_ANGLE_UNIT ( ) SI_UNIT ( $, .RADIAN. ) );
#13563 = EDGE_LOOP ( 'NONE', ( #13281, #4974, #886, #2145 ) ) ;
#13564 = FACE_OUTER_BOUND ( 'NONE', #14796, .T. ) ;
#13565 = AXIS2_PLACEMENT_3D ( 'NONE', #232, #13939, #15167 ) ;
#13566 = ORIENTED_EDGE ( 'NONE', *, *, #4725, .T. ) ;
#13567 = CARTESIAN_POINT ( 'NONE',  ( 4.729367062499999719, -21.84375000068279604, 0.000000000000000000 ) ) ;
#13568 = CIRCLE ( 'NONE', #9468, 3.499999999999999556 ) ;
#13569 = CARTESIAN_POINT ( 'NONE',  ( -21.01110699893060030, 0.000000000000000000, 36.39230484541324273 ) ) ;
#13570 = ADVANCED_FACE ( 'NONE', ( #7823 ), #6601, .F. ) ;
#13571 = B_SPLINE_CURVE_WITH_KNOTS ( 'NONE', 3,
 ( #15557, #10554, #4474, #14006 ),
 .UNSPECIFIED., .F., .F.,
 ( 4, 4 ),
 ( 0.000000000000000000, 0.002452478801916376308 ),
 .UNSPECIFIED. ) ;
#13572 = CARTESIAN_POINT ( 'NONE',  ( -0.5093500532425060401, -4.799145180956616130, -3.624999998634407916 ) ) ;
#13573 = EDGE_CURVE ( 'NONE', #6357, #2056, #2629, .T. ) ;
#13574 = APPLICATION_PROTOCOL_DEFINITION ( 'draft international standard', 'automotive_design', 1998, #14240 ) ;
#13575 = AXIS2_PLACEMENT_3D ( 'NONE', #15123, #2836, #7788 ) ;
#13576 = CARTESIAN_POINT ( 'NONE',  ( 3.916244202832140253, -2.131511515620588160, -3.687499998634407916 ) ) ;
#13577 = CIRCLE ( 'NONE', #14377, 5.999999999999991118 ) ;
#13578 = DIRECTION ( 'NONE',  ( 0.000000000000000000, 1.000000000000000000, 0.000000000000000000 ) ) ;
#13579 = CARTESIAN_POINT ( 'NONE',  ( -15.99999999999979217, -9.000000000000001776, 1.499999999999998890 ) ) ;
#13580 = ORIENTED_EDGE ( 'NONE', *, *, #5244, .F. ) ;
#13581 = CARTESIAN_POINT ( 'NONE',  ( 4.896370289182463864, -4.865128266864630291, -48.48076211353469489 ) ) ;
#13582 = PRESENTATION_STYLE_ASSIGNMENT (( #14569 ) ) ;
#13583 = EDGE_LOOP ( 'NONE', ( #11594, #11919, #6623, #9765 ) ) ;
#13584 = CARTESIAN_POINT ( 'NONE',  ( -91.33974596215558961, -105.7735026918962404, 17.50000000000000000 ) ) ;
#13585 = CIRCLE ( 'NONE', #15684, 2.041999999999999815 ) ;
#13586 = VERTEX_POINT ( 'NONE', #1337 ) ;
#13587 = VERTEX_POINT ( 'NONE', #6284 ) ;
#13588 = ITEM_DEFINED_TRANSFORMATION ( 'NONE', 'NONE', #1926,  #3223 ) ;
#13589 = CARTESIAN_POINT ( 'NONE',  ( 0.5093500532425063732, 4.799145180956616130, -2.374999998634407028 ) ) ;
#13590 = CARTESIAN_POINT ( 'NONE',  ( -21.01110699893041911, -3.000000000000000000, -36.39230484541334221 ) ) ;
#13591 = CARTESIAN_POINT ( 'NONE',  ( 4.276409079477644148, 1.261996585732577891, -8.562499998634409692 ) ) ;
#13592 = AXIS2_PLACEMENT_3D ( 'NONE', #14, #3551, #11148 ) ;
#13593 = CARTESIAN_POINT ( 'NONE',  ( 5.200000000000002842, 0.000000000000000000, 0.000000000000000000 ) ) ;
#13594 = VECTOR ( 'NONE', #13128, 1000.000000000000000 ) ;
#13595 = ADVANCED_FACE ( 'NONE', ( #11197 ), #143, .T. ) ;
#13596 = PRODUCT_RELATED_PRODUCT_CATEGORY ( 'part', '', ( #609 ) ) ;
#13597 = CARTESIAN_POINT ( 'NONE',  ( -55.00000000000000000, -1.982541115402065307E-15, -7.500000000000000000 ) ) ;
#13598 = CARTESIAN_POINT ( 'NONE',  ( 4.209348295687701302, 3.401574460001765665, -4.812499997268817609 ) ) ;
#13599 = DIRECTION ( 'NONE',  ( 0.000000000000000000, 0.000000000000000000, -1.000000000000000000 ) ) ;
#13600 = LINE ( 'NONE', #13929, #6942 ) ;
#13601 = CARTESIAN_POINT ( 'NONE',  ( 4.458734124999999437, -24.68750000136559564, 0.000000000000000000 ) ) ;
#13602 = ORIENTED_EDGE ( 'NONE', *, *, #2102, .F. ) ;
#13604 = B_SPLINE_CURVE_WITH_KNOTS ( 'NONE', 3,
 ( #3114, #4325, #9337, #10469, #12876, #6997 ),
 .UNSPECIFIED., .F., .F.,
 ( 4, 2, 4 ),
 ( -5.145455527297706927E-06, 0.0004153350442917282375, 0.0008358155441107520661 ),
 .UNSPECIFIED. ) ;
#13603 = CARTESIAN_POINT ( 'NONE',  ( -4.458734125000000326, -23.87500000136559564, 1.846868145590734089 ) ) ;
#13605 = CARTESIAN_POINT ( 'NONE',  ( 3.033343224707661712, -3.753672977998669946, -5.499999998634407916 ) ) ;
#13606 = CONICAL_SURFACE ( 'NONE', #8990, 7.500000000000001776, 0.8594454914424796144 ) ;
#13607 = DIRECTION ( 'NONE',  ( -0.000000000000000000, 1.000000000000000000, -0.000000000000000000 ) ) ;
#13608 = ORIENTED_EDGE ( 'NONE', *, *, #11856, .F. ) ;
#13609 = VERTEX_POINT ( 'NONE', #12562 ) ;
#13610 = SURFACE_STYLE_FILL_AREA ( #7496 ) ;
#13611 = VERTEX_POINT ( 'NONE', #9038 ) ;
#13612 = CARTESIAN_POINT ( 'NONE',  ( -4.458734124999999437, -24.18750000136559564, -5.460374474430324690E-16 ) ) ;
#13613 = CARTESIAN_POINT ( 'NONE',  ( -35.00000000000000000, 50.00000000000000000, 0.000000000000000000 ) ) ;
#13614 = LINE ( 'NONE', #15082, #660 ) ;
#13615 = EDGE_CURVE ( 'NONE', #7701, #7037, #8146, .T. ) ;
#13616 = PLANE ( 'NONE',  #6384 ) ;
#13617 = CARTESIAN_POINT ( 'NONE',  ( 0.000000000000000000, 0.000000000000000000, 0.000000000000000000 ) ) ;
#13618 = EDGE_CURVE ( 'NONE', #6321, #13119, #12645, .T. ) ;
#13619 = ADVANCED_FACE ( 'NONE', ( #9997 ), #14933, .F. ) ;
#13620 = EDGE_CURVE ( 'NONE', #8118, #10581, #3725, .T. ) ;
#13621 = CARTESIAN_POINT ( 'NONE',  ( -28.86751345948126612, -4.999999999999997335, -20.00000000000000355 ) ) ;
#13622 = CARTESIAN_POINT ( 'NONE',  ( -5.381735091635034607, 0.5711823568785950878, 0.4374999999999975020 ) ) ;
#13623 = CARTESIAN_POINT ( 'NONE',  ( -21.01110699893041556, -1.230770033143087371E-15, -36.39230484541334221 ) ) ;
#13624 = VECTOR ( 'NONE', #8381, 1000.000000000000000 ) ;
#13625 = CYLINDRICAL_SURFACE ( 'NONE', #14664, 1.999999999999998224 ) ;
#13626 = CARTESIAN_POINT ( 'NONE',  ( 1.846868145590735200, -28.25000000136559208, -4.458734125000000326 ) ) ;
#13627 = PRESENTATION_LAYER_ASSIGNMENT (  '', '', ( #3323 ) ) ;
#13628 = CARTESIAN_POINT ( 'NONE',  ( 2.131511515620586383, 3.916244202832140253, -4.437499998634405252 ) ) ;
#13629 = ORIENTED_EDGE ( 'NONE', *, *, #3102, .F. ) ;
#13630 = CARTESIAN_POINT ( 'NONE',  ( 2.500000000000000000, 1.178949249685213863, -2.042000000000001148 ) ) ;
#13631 = ORIENTED_EDGE ( 'NONE', *, *, #14088, .T. ) ;
#13632 = ORIENTED_EDGE ( 'NONE', *, *, #1343, .F. ) ;
#13633 = FACE_OUTER_BOUND ( 'NONE', #8114, .T. ) ;
#13634 = AXIS2_PLACEMENT_3D ( 'NONE', #11328, #10120, #5265 ) ;
#13635 = CARTESIAN_POINT ( 'NONE',  ( 3.152801135295367541, -26.31250000136559564, -3.152801135295367541 ) ) ;
#13636 = CARTESIAN_POINT ( 'NONE',  ( -6.765421556309547668E-13, 40.00000000000000000, 67.49999999999930367 ) ) ;
#13637 = VERTEX_POINT ( 'NONE', #6365 ) ;
#13638 = CARTESIAN_POINT ( 'NONE',  ( 23.49999999999956657, -8.786575603324269439E-13, -11.50000000000000000 ) ) ;
#13639 = AXIS2_PLACEMENT_3D ( 'NONE', #3243, #14166, #8191 ) ;
#13640 = VECTOR ( 'NONE', #15840, 1000.000000000000000 ) ;
#13641 = DIRECTION ( 'NONE',  ( 1.000000000000000000, 0.000000000000000000, 0.000000000000000000 ) ) ;
#13642 = DIRECTION ( 'NONE',  ( 0.000000000000000000, 1.000000000000000000, 0.000000000000000000 ) ) ;
#13643 = DIRECTION ( 'NONE',  ( -1.000000000000000000, -0.000000000000000000, -0.000000000000000000 ) ) ;
#13644 = EDGE_CURVE ( 'NONE', #7371, #9203, #2708, .T. ) ;
#13645 = CARTESIAN_POINT ( 'NONE',  ( 3.535533905932736864, -31.12500000000000000, 3.535533905932738641 ) ) ;
#13646 = CARTESIAN_POINT ( 'NONE',  ( -6.765421556309547668E-13, 40.00000000000000000, 70.14999999999929514 ) ) ;
#13647 = CARTESIAN_POINT ( 'NONE',  ( 6.000000000000000000, -13.00000000000000178, 1.500000000000000000 ) ) ;
#13648 = CARTESIAN_POINT ( 'NONE',  ( -5.000000000000000888, -26.68750000273119127, -2.071067811865475949 ) ) ;
#13649 = CARTESIAN_POINT ( 'NONE',  ( -60.00000000000000000, -35.00000000000000000, 19.99999999999999289 ) ) ;
#13650 = CARTESIAN_POINT ( 'NONE',  ( -4.458734124999999437, -30.00000000136559919, -1.846868145590735644 ) ) ;
#13651 = EDGE_LOOP ( 'NONE', ( #2534, #5768 ) ) ;
#13652 = EDGE_LOOP ( 'NONE', ( #10239, #7269, #5318 ) ) ;
#13653 = VECTOR ( 'NONE', #676, 1000.000000000000000 ) ;
#13654 =( NAMED_UNIT ( * ) PLANE_ANGLE_UNIT ( ) SI_UNIT ( $, .RADIAN. ) );
#13655 = ORIENTED_EDGE ( 'NONE', *, *, #5000, .T. ) ;
#13656 = DIRECTION ( 'NONE',  ( -0.5000000000000051070, 0.000000000000000000, 0.8660254037844355990 ) ) ;
#13657 =( BOUNDED_SURFACE ( )  B_SPLINE_SURFACE ( 1, 2, ( 
 ( #13336, #14415, #5758, #14649, #12201, #3341, #5841, #3258, #6081, #8205, #10695, #9627, #13416, #11011, #15630, #2043, #4549, #7064, #15950, #14562, #11888, #4873, #6001, #12048, #4786, #11965, #14331, #8522, #3571, #13104, #6989, #9483, #13253, #8443, #13179, #2115, #8289, #916, #2194, #10777, #15715, #14487, #3409, #8360, #2278, #7145, #1065, #993, #5927, #10849, #15789, #4706, #7230, #10925, #9711, #9138, #13661, #3650, #5334, #6328, #7376, #104, #14050, #14727, #12285, #1222, #2423, #9800, #11245, #9874, #6247, #6170, #10351, #8595, #11093, #29, #4945, #13485, #192, #14805, #11161, #3727, #15278, #10272, #8671, #13572, #11543, #5023, #2503, #13965, #7464, #12369, #9952, #1302, #7931, #14891, #3811, #8759, #7544, #2591, #12445, #1379, #15200, #4115, #4192, #12827, #9063, #2897, #2977, #7847, #12745, #6718, #1771, #1690, #6631, #495, #5419, #11621, #571, #11695, #3144, #2085, #8091, #650, #729, #9528, #3378, #805, #5655, #11777, #9447, #15520, #14457, #8013, #5492, #5574, #15444, #15593, #4512, #10511, #12909, #5800, #8329, #4366, #12985, #10422, #13219, #15357, #1844, #5725, #4590, #2158, #6787, #9218, #9300, #14223, #7107, #10660, #3070, #12009, #13150 ),
 ( #10596, #14378, #1921, #4277, #6870, #2007, #7030, #3304, #4436, #9371, #14296, #3219, #14140, #11930, #8258, #8168, #882, #13070, #6957, #11858, #10739, #15676, #3615, #8560, #4909, #13622, #8402, #11126, #9910, #1032, #14531, #14767, #2320, #6212, #67, #8636, #2758, #3771, #12092, #14693, #13449, #5967, #2389, #10888, #12243, #4670, #14850, #7425, #15829, #2553, #13382, #6129, #4985, #4749, #9669, #4831, #3449, #9594, #1267, #7506, #13294, #960, #7338, #9835, #14607, #7192, #13530, #9755, #3689, #1103, #1184, #2465, #10819, #8716, #8481, #7264, #12330, #3528, #5885, #2236, #15759, #12165, #6043, #10968, #11055, #15910, #5228, #6371, #8958, #2633, #2877, #9118, #7584, #5069, #13869, #1424, #2954, #8874, #1341, #12725, #12649, #13946, #2801, #4170, #3858, #12407, #1664, #12484, #11205, #14025, #6290, #1516, #6527, #3929, #149, #11289, #7758, #4092, #11442, #13778, #6454, #11366, #239, #10001, #7828, #10248, #471, #1588, #15259, #5395, #14938, #7671, #8797, #15088, #4005, #389, #13701, #5158, #6606, #10333, #10088, #15015, #15176, #2713, #11521, #12569, #318, #5308, #10164, #9043, #859, #5779, #10720, #553, #4417, #1824, #14202, #9507, #4572, #12805, #15654 ) ),
 .UNSPECIFIED., .F., .F., .F. ) 
 B_SPLINE_SURFACE_WITH_KNOTS ( ( 2, 2 ),
 ( 3, 2, 2, 2, 2, 2, 2, 2, 2, 2, 2, 2, 2, 2, 2, 2, 2, 2, 2, 2, 2, 2, 2, 2, 2, 2, 2, 2, 2, 2, 2, 2, 2, 2, 2, 2, 2, 2, 2, 2, 2, 2, 2, 2, 2, 2, 2, 2, 2, 2, 2, 2, 2, 2, 2, 2, 2, 2, 2, 2, 2, 2, 2, 2, 2, 2, 2, 2, 2, 2, 2, 2, 2, 2, 2, 2, 2, 2, 2, 2, 3 ),
 ( 0.000000000000000000, 1.000000000000000000 ),
 ( 0.000000000000000000, 0.01250000000000000069, 0.02500000000000000139, 0.03749999999999999861, 0.05000000000000000278, 0.06250000000000000000, 0.07499999999999999722, 0.08749999999999999445, 0.1000000000000000056, 0.1125000000000000028, 0.1250000000000000000, 0.1375000000000000111, 0.1499999999999999944, 0.1625000000000000056, 0.1749999999999999889, 0.1875000000000000000, 0.2000000000000000111, 0.2124999999999999944, 0.2250000000000000056, 0.2374999999999999889, 0.2500000000000000000, 0.2625000000000000111, 0.2750000000000000222, 0.2874999999999999778, 0.2999999999999999889, 0.3125000000000000000, 0.3250000000000000111, 0.3375000000000000222, 0.3499999999999999778, 0.3624999999999999889, 0.3750000000000000000, 0.3875000000000000111, 0.4000000000000000222, 0.4124999999999999778, 0.4249999999999999889, 0.4375000000000000000, 0.4500000000000000111, 0.4625000000000000222, 0.4749999999999999778, 0.4874999999999999889, 0.5000000000000000000, 0.5124999999999999556, 0.5250000000000000222, 0.5374999999999999778, 0.5500000000000000444, 0.5625000000000000000, 0.5749999999999999556, 0.5875000000000000222, 0.5999999999999999778, 0.6125000000000000444, 0.6250000000000000000, 0.6374999999999999556, 0.6500000000000000222, 0.6624999999999999778, 0.6750000000000000444, 0.6875000000000000000, 0.6999999999999999556, 0.7125000000000000222, 0.7249999999999999778, 0.7375000000000000444, 0.7500000000000000000, 0.7624999999999999556, 0.7750000000000000222, 0.7874999999999999778, 0.8000000000000000444, 0.8125000000000000000, 0.8249999999999999556, 0.8375000000000000222, 0.8499999999999999778, 0.8625000000000000444, 0.8750000000000000000, 0.8874999999999999556, 0.9000000000000000222, 0.9124999999999999778, 0.9250000000000000444, 0.9375000000000000000, 0.9499999999999999556, 0.9625000000000000222, 0.9749999999999999778, 0.9875000000000000444, 1.000000000000000000 ),
 .UNSPECIFIED. ) 
 GEOMETRIC_REPRESENTATION_ITEM ( )  RATIONAL_B_SPLINE_SURFACE ( (
 ( 1.000000000000000000, 0.9238795325112867385, 1.000000000000000000, 0.9238795325112867385, 1.000000000000000000, 0.9238795325112867385, 1.000000000000000000, 0.9238795325112867385, 1.000000000000000000, 0.9238795325112867385, 1.000000000000000000, 0.9238795325112867385, 1.000000000000000000, 0.9238795325112867385, 1.000000000000000000, 0.9238795325112867385, 1.000000000000000000, 0.9238795325112867385, 1.000000000000000000, 0.9238795325112867385, 1.000000000000000000, 0.9238795325112867385, 1.000000000000000000, 0.9238795325112867385, 1.000000000000000000, 0.9238795325112867385, 1.000000000000000000, 0.9238795325112867385, 1.000000000000000000, 0.9238795325112867385, 1.000000000000000000, 0.9238795325112867385, 1.000000000000000000, 0.9238795325112867385, 1.000000000000000000, 0.9238795325112867385, 1.000000000000000000, 0.9238795325112867385, 1.000000000000000000, 0.9238795325112867385, 1.000000000000000000, 0.9238795325112867385, 1.000000000000000000, 0.9238795325112867385, 1.000000000000000000, 0.9238795325112867385, 1.000000000000000000, 0.9238795325112867385, 1.000000000000000000, 0.9238795325112867385, 1.000000000000000000, 0.9238795325112867385, 1.000000000000000000, 0.9238795325112867385, 1.000000000000000000, 0.9238795325112867385, 1.000000000000000000, 0.9238795325112867385, 1.000000000000000000, 0.9238795325112867385, 1.000000000000000000, 0.9238795325112867385, 1.000000000000000000, 0.9238795325112867385, 1.000000000000000000, 0.9238795325112867385, 1.000000000000000000, 0.9238795325112867385, 1.000000000000000000, 0.9238795325112867385, 1.000000000000000000, 0.9238795325112867385, 1.000000000000000000, 0.9238795325112867385, 1.000000000000000000, 0.9238795325112867385, 1.000000000000000000, 0.9238795325112867385, 1.000000000000000000, 0.9238795325112867385, 1.000000000000000000, 0.9238795325112867385, 1.000000000000000000, 0.9238795325112867385, 1.000000000000000000, 0.9238795325112867385, 1.000000000000000000, 0.9238795325112867385, 1.000000000000000000, 0.9238795325112867385, 1.000000000000000000, 0.9238795325112867385, 1.000000000000000000, 0.9238795325112867385, 1.000000000000000000, 0.9238795325112867385, 1.000000000000000000, 0.9238795325112867385, 1.000000000000000000, 0.9238795325112867385, 1.000000000000000000, 0.9238795325112867385, 1.000000000000000000, 0.9238795325112867385, 1.000000000000000000, 0.9238795325112867385, 1.000000000000000000, 0.9238795325112867385, 1.000000000000000000, 0.9238795325112867385, 1.000000000000000000, 0.9238795325112867385, 1.000000000000000000, 0.9238795325112867385, 1.000000000000000000, 0.9238795325112867385, 1.000000000000000000, 0.9238795325112867385, 1.000000000000000000, 0.9238795325112867385, 1.000000000000000000, 0.9238795325112867385, 1.000000000000000000, 0.9238795325112867385, 1.000000000000000000, 0.9238795325112867385, 1.000000000000000000, 0.9238795325112867385, 1.000000000000000000, 0.9238795325112867385, 1.000000000000000000, 0.9238795325112867385, 1.000000000000000000, 0.9238795325112867385, 1.000000000000000000, 0.9238795325112867385, 1.000000000000000000, 0.9238795325112867385, 1.000000000000000000, 0.9238795325112867385, 1.000000000000000000, 0.9238795325112867385, 1.000000000000000000, 0.9238795325112867385, 1.000000000000000000, 0.9238795325112867385, 1.000000000000000000, 0.9238795325112867385, 1.000000000000000000, 0.9238795325112867385, 1.000000000000000000, 0.9238795325112867385, 1.000000000000000000, 0.9238795325112867385, 1.000000000000000000, 0.9238795325112867385, 1.000000000000000000, 0.9238795325112867385, 1.000000000000000000, 0.9238795325112867385, 1.000000000000000000),
 ( 1.000000000000000000, 0.9238795325112867385, 1.000000000000000000, 0.9238795325112867385, 1.000000000000000000, 0.9238795325112867385, 1.000000000000000000, 0.9238795325112867385, 1.000000000000000000, 0.9238795325112867385, 1.000000000000000000, 0.9238795325112867385, 1.000000000000000000, 0.9238795325112867385, 1.000000000000000000, 0.9238795325112867385, 1.000000000000000000, 0.9238795325112867385, 1.000000000000000000, 0.9238795325112867385, 1.000000000000000000, 0.9238795325112867385, 1.000000000000000000, 0.9238795325112867385, 1.000000000000000000, 0.9238795325112867385, 1.000000000000000000, 0.9238795325112867385, 1.000000000000000000, 0.9238795325112867385, 1.000000000000000000, 0.9238795325112867385, 1.000000000000000000, 0.9238795325112867385, 1.000000000000000000, 0.9238795325112867385, 1.000000000000000000, 0.9238795325112867385, 1.000000000000000000, 0.9238795325112867385, 1.000000000000000000, 0.9238795325112867385, 1.000000000000000000, 0.9238795325112867385, 1.000000000000000000, 0.9238795325112867385, 1.000000000000000000, 0.9238795325112867385, 1.000000000000000000, 0.9238795325112867385, 1.000000000000000000, 0.9238795325112867385, 1.000000000000000000, 0.9238795325112867385, 1.000000000000000000, 0.9238795325112867385, 1.000000000000000000, 0.9238795325112867385, 1.000000000000000000, 0.9238795325112867385, 1.000000000000000000, 0.9238795325112867385, 1.000000000000000000, 0.9238795325112867385, 1.000000000000000000, 0.9238795325112867385, 1.000000000000000000, 0.9238795325112867385, 1.000000000000000000, 0.9238795325112867385, 1.000000000000000000, 0.9238795325112867385, 1.000000000000000000, 0.9238795325112867385, 1.000000000000000000, 0.9238795325112867385, 1.000000000000000000, 0.9238795325112867385, 1.000000000000000000, 0.9238795325112867385, 1.000000000000000000, 0.9238795325112867385, 1.000000000000000000, 0.9238795325112867385, 1.000000000000000000, 0.9238795325112867385, 1.000000000000000000, 0.9238795325112867385, 1.000000000000000000, 0.9238795325112867385, 1.000000000000000000, 0.9238795325112867385, 1.000000000000000000, 0.9238795325112867385, 1.000000000000000000, 0.9238795325112867385, 1.000000000000000000, 0.9238795325112867385, 1.000000000000000000, 0.9238795325112867385, 1.000000000000000000, 0.9238795325112867385, 1.000000000000000000, 0.9238795325112867385, 1.000000000000000000, 0.9238795325112867385, 1.000000000000000000, 0.9238795325112867385, 1.000000000000000000, 0.9238795325112867385, 1.000000000000000000, 0.9238795325112867385, 1.000000000000000000, 0.9238795325112867385, 1.000000000000000000, 0.9238795325112867385, 1.000000000000000000, 0.9238795325112867385, 1.000000000000000000, 0.9238795325112867385, 1.000000000000000000, 0.9238795325112867385, 1.000000000000000000, 0.9238795325112867385, 1.000000000000000000, 0.9238795325112867385, 1.000000000000000000, 0.9238795325112867385, 1.000000000000000000, 0.9238795325112867385, 1.000000000000000000, 0.9238795325112867385, 1.000000000000000000, 0.9238795325112867385, 1.000000000000000000, 0.9238795325112867385, 1.000000000000000000, 0.9238795325112867385, 1.000000000000000000, 0.9238795325112867385, 1.000000000000000000, 0.9238795325112867385, 1.000000000000000000, 0.9238795325112867385, 1.000000000000000000, 0.9238795325112867385, 1.000000000000000000, 0.9238795325112867385, 1.000000000000000000, 0.9238795325112867385, 1.000000000000000000, 0.9238795325112867385, 1.000000000000000000, 0.9238795325112867385, 1.000000000000000000, 0.9238795325112867385, 1.000000000000000000, 0.9238795325112867385, 1.000000000000000000, 0.9238795325112867385, 1.000000000000000000) ) ) 
 REPRESENTATION_ITEM ( '' )  SURFACE ( )  );
#13658 = ORIENTED_EDGE ( 'NONE', *, *, #11261, .T. ) ;
#13659 = CARTESIAN_POINT ( 'NONE',  ( 39.53738644056436868, -5.000000000000000000, 28.48076211354233322 ) ) ;
#13660 = CARTESIAN_POINT ( 'NONE',  ( -4.458734124999999437, -31.18750000136559564, -5.460374474430324690E-16 ) ) ;
#13661 = CARTESIAN_POINT ( 'NONE',  ( -4.276409079477644148, -1.261996585732578335, -1.812499998634406584 ) ) ;
#13662 = SHAPE_DEFINITION_REPRESENTATION ( #15846, #3173 ) ;
#13663 = CARTESIAN_POINT ( 'NONE',  ( -3.033343224707664376, 3.753672977998667726, -6.249999998634408804 ) ) ;
#13664 = DIRECTION ( 'NONE',  ( 0.8660254037844388186, -0.000000000000000000, -0.4999999999999998890 ) ) ;
#13665 = CARTESIAN_POINT ( 'NONE',  ( 3.535533905932738197, -23.87500000000000000, -3.535533905932738197 ) ) ;
#13666 = ORIENTED_EDGE ( 'NONE', *, *, #13696, .T. ) ;
#13667 = CARTESIAN_POINT ( 'NONE',  ( -7.500000000000005329, 2.886751345948128655, -7.198902722707430257 ) ) ;
#13668 = FILL_AREA_STYLE ('',( #3821 ) ) ;
#13669 = VERTEX_POINT ( 'NONE', #7665 ) ;
#13670 = CARTESIAN_POINT ( 'NONE',  ( 4.211399257449709665, -2.459727064652517114, -3.751161691472417736 ) ) ;
#13671 = CARTESIAN_POINT ( 'NONE',  ( 4.458734124999999437, -21.43750000136559208, 0.000000000000000000 ) ) ;
#13672 = EDGE_LOOP ( 'NONE', ( #4660, #9880, #2472, #10534 ) ) ;
#13673 = ITEM_DEFINED_TRANSFORMATION ( 'NONE', 'NONE', #125,  #3223 ) ;
#13674 = CARTESIAN_POINT ( 'NONE',  ( 1.261996585732578113, -4.276409079477644148, -5.812499998634406140 ) ) ;
#13675 = ADVANCED_FACE ( 'NONE', ( #549 ), #4487, .T. ) ;
#13676 = FACE_OUTER_BOUND ( 'NONE', #9866, .T. ) ;
#13677 = CARTESIAN_POINT ( 'NONE',  ( 1.261996585732578113, -4.276409079477644148, -7.562499998634407916 ) ) ;
#13678 = LINE ( 'NONE', #3981, #3021 ) ;
#13679 = PRODUCT_DEFINITION_CONTEXT ( 'detailed design', #12991, 'design' ) ;
#13680 = CARTESIAN_POINT ( 'NONE',  ( 3.535533905932736864, -27.25000000273118772, 3.535533905932738641 ) ) ;
#13681 = CARTESIAN_POINT ( 'NONE',  ( 4.391654775818395251, -2.390265326283149694, -4.999999997268817609 ) ) ;
#13682 = CARTESIAN_POINT ( 'NONE',  ( 6.000000000000000000, -13.00000000000000178, -1.500000000000000000 ) ) ;
#13683 = DIRECTION ( 'NONE',  ( 1.000000000000000000, 0.000000000000000000, 0.000000000000000000 ) ) ;
#13684 = CARTESIAN_POINT ( 'NONE',  ( 2.730187237215162345E-16, -25.43750000136559564, -4.458734124999999437 ) ) ;
#13685 = ORIENTED_EDGE ( 'NONE', *, *, #1043, .T. ) ;
#13686 = DIRECTION ( 'NONE',  ( -1.000000000000000000, -0.000000000000000000, -0.000000000000000000 ) ) ;
#13687 = CARTESIAN_POINT ( 'NONE',  ( -1.261996585732579224, 4.276409079477648589, -7.062499998634407916 ) ) ;
#13688 = LINE ( 'NONE', #15003, #12261 ) ;
#13689 = EDGE_LOOP ( 'NONE', ( #12903, #1172, #15941, #14363, #1414 ) ) ;
#13690 = VERTEX_POINT ( 'NONE', #9189 ) ;
#13691 = DIRECTION ( 'NONE',  ( 0.000000000000000000, 0.000000000000000000, 1.000000000000000000 ) ) ;
#13692 = ORIENTED_EDGE ( 'NONE', *, *, #6122, .T. ) ;
#13693 = CARTESIAN_POINT ( 'NONE',  ( -3.152801135295367096, -22.31250000136559564, -3.152801135295367541 ) ) ;
#13694 = EDGE_CURVE ( 'NONE', #4036, #15708, #1837, .T. ) ;
#13695 = DIRECTION ( 'NONE',  ( 0.9999824063907752913, 0.005931855436078211502, -0.000000000000000000 ) ) ;
#13696 = EDGE_CURVE ( 'NONE', #9210, #7197, #5280, .T. ) ;
#13697 = CARTESIAN_POINT ( 'NONE',  ( -67.50000000000000000, 50.00000000000000000, -7.070249711157346244E-13 ) ) ;
#13698 = DIRECTION ( 'NONE',  ( -1.000000000000000000, -0.000000000000000000, -0.000000000000000000 ) ) ;
#13699 = PLANE ( 'NONE',  #8086 ) ;
#13700 = DIRECTION ( 'NONE',  ( -1.000000000000000000, -0.000000000000000000, -0.000000000000000000 ) ) ;
#13701 = CARTESIAN_POINT ( 'NONE',  ( -4.795541693661363958, -1.415196051561583790, -6.500000000000002665 ) ) ;
#13702 = DIRECTION ( 'NONE',  ( -1.000000000000000000, 0.000000000000000000, 0.000000000000000000 ) ) ;
#13703 = CARTESIAN_POINT ( 'NONE',  ( -4.175002511812151873, -2.208363329454905877, -3.469254087858246738 ) ) ;
#13704 = CARTESIAN_POINT ( 'NONE',  ( 3.152801135295366208, -28.56250000136559564, 3.152801135295367985 ) ) ;
#13705 = CARTESIAN_POINT ( 'NONE',  ( -1.261996585732579224, 4.276409079477648589, -1.312499998634406140 ) ) ;
#13706 = ORIENTED_EDGE ( 'NONE', *, *, #2772, .T. ) ;
#13707 = LINE ( 'NONE', #7432, #15633 ) ;
#13708 = ORIENTED_EDGE ( 'NONE', *, *, #7005, .T. ) ;
#13709 = ORIENTED_EDGE ( 'NONE', *, *, #1176, .T. ) ;
#13710 = CARTESIAN_POINT ( 'NONE',  ( 0.000000000000000000, -20.00000000000000000, 5.000000000000000000 ) ) ;
#13711 = CARTESIAN_POINT ( 'NONE',  ( -4.458734124999999437, -23.93750000136559564, -5.460374474430324690E-16 ) ) ;
#13712 = ADVANCED_FACE ( 'NONE', ( #4334, #10478 ), #7900, .T. ) ;
#13713 = DIRECTION ( 'NONE',  ( -1.000000000000000000, -0.000000000000000000, -0.000000000000000000 ) ) ;
#13714 = EDGE_CURVE ( 'NONE', #10675, #15345, #5796, .T. ) ;
#13715 = ORIENTED_EDGE ( 'NONE', *, *, #8998, .T. ) ;
#13716 = CARTESIAN_POINT ( 'NONE',  ( 2.725741868436127202, -3.045094352033990148, -3.220599429844051453 ) ) ;
#13717 = DIRECTION ( 'NONE',  ( 0.000000000000000000, 0.000000000000000000, -1.000000000000000000 ) ) ;
#13718 = CARTESIAN_POINT ( 'NONE',  ( -3.753672977998669502, -3.033343224707661712, -0.7499999986344074721 ) ) ;
#13719 = CARTESIAN_POINT ( 'NONE',  ( 0.5789871446316211534, 4.420982230657665824, -0.3789984458506777676 ) ) ;
#13720 = CARTESIAN_POINT ( 'NONE',  ( 2.071067811865475505, -31.81250000000000000, -5.000000000000000888 ) ) ;
#13721 = CARTESIAN_POINT ( 'NONE',  ( 35.00000000000000000, 37.00000000000000000, -2.649999999999994582 ) ) ;
#13722 = CARTESIAN_POINT ( 'NONE',  ( -67.50000000000000000, 50.00000000000000000, -2.650000000000699352 ) ) ;
#13723 = CARTESIAN_POINT ( 'NONE',  ( -2.071067811865478170, -26.43750000273119127, 5.000000000000000000 ) ) ;
#13724 = DIRECTION ( 'NONE',  ( -0.000000000000000000, -1.000000000000000000, -0.000000000000000000 ) ) ;
#13725 = CARTESIAN_POINT ( 'NONE',  ( 1.846868145590736310, -28.62500000136559564, 4.458734124999997661 ) ) ;
#13726 = LINE ( 'NONE', #12360, #1949 ) ;
#13727 = ORIENTED_EDGE ( 'NONE', *, *, #14920, .T. ) ;
#13728 = VERTEX_POINT ( 'NONE', #11832 ) ;
#13729 = VECTOR ( 'NONE', #6175, 1000.000000000000000 ) ;
#13730 = ORIENTED_EDGE ( 'NONE', *, *, #6241, .T. ) ;
#13731 = AXIS2_PLACEMENT_3D ( 'NONE', #12983, #6867, #4509 ) ;
#13732 = LINE ( 'NONE', #5186, #11491 ) ;
#13733 = EDGE_CURVE ( 'NONE', #12492, #1994, #7876, .T. ) ;
#13734 = ORIENTED_EDGE ( 'NONE', *, *, #1383, .T. ) ;
#13735 = CARTESIAN_POINT ( 'NONE',  ( 7.894787914004607998, -0.7647108141804138670, -7.591390474663419319 ) ) ;
#13736 = CARTESIAN_POINT ( 'NONE',  ( -5.000000000000004441, -1.011557177027151181E-15, -4.420263044861760804 ) ) ;
#13737 = AXIS2_PLACEMENT_3D ( 'NONE', #2820, #491, #4113 ) ;
#13738 = SHAPE_DEFINITION_REPRESENTATION ( #4738, #790 ) ;
#13739 = CARTESIAN_POINT ( 'NONE',  ( -3.753672977998669946, -3.033343224707661712, -6.999999998634408804 ) ) ;
#13740 = DIRECTION ( 'NONE',  ( 0.000000000000000000, 1.000000000000000000, 0.000000000000000000 ) ) ;
#13741 = CYLINDRICAL_SURFACE ( 'NONE', #8488, 5.000000000000001776 ) ;
#13742 = ORIENTED_EDGE ( 'NONE', *, *, #119, .T. ) ;
#13743 =( BOUNDED_CURVE ( )  B_SPLINE_CURVE ( 2, ( #6206, #7498, #9902, #1335, #6281 ),
 .UNSPECIFIED., .F., .F. ) 
 B_SPLINE_CURVE_WITH_KNOTS ( ( 3, 2, 3 ),
 ( 0.000000000000000000, 0.01250000000000001110, 0.02500000000000002220 ),
 .UNSPECIFIED. ) 
 CURVE ( )  GEOMETRIC_REPRESENTATION_ITEM ( )  RATIONAL_B_SPLINE_CURVE ( ( 1.000000000000000000, 0.9238795325112867385, 1.000000000000000000, 0.9238795325112866275, 1.000000000000000222 ) ) 
 REPRESENTATION_ITEM ( '' )  );
#13744 = CARTESIAN_POINT ( 'NONE',  ( 57.73502691896258199, 1.999999999999998224, 2.081668171172168513E-14 ) ) ;
#13745 = AXIS2_PLACEMENT_3D ( 'NONE', #6291, #4986, #9836 ) ;
#13746 = APPLICATION_PROTOCOL_DEFINITION ( 'draft international standard', 'automotive_design', 1998, #8162 ) ;
#13747 = ORIENTED_EDGE ( 'NONE', *, *, #6490, .F. ) ;
#13748 = DIRECTION ( 'NONE',  ( 1.000000000000000000, 1.734723475976808080E-16, 0.000000000000000000 ) ) ;
#13749 = CARTESIAN_POINT ( 'NONE',  ( 0.000000000000000000, 0.000000000000000000, 0.000000000000000000 ) ) ;
#13750 = EDGE_CURVE ( 'NONE', #6730, #11426, #2952, .T. ) ;
#13751 = EDGE_LOOP ( 'NONE', ( #3079, #13992, #56, #10862 ) ) ;
#13752 = CARTESIAN_POINT ( 'NONE',  ( 3.033343224707661712, -3.753672977998669502, -5.749999998634407916 ) ) ;
#13753 = B_SPLINE_CURVE_WITH_KNOTS ( 'NONE', 3,
 ( #5981, #13237, #14544, #3393, #7124, #9688 ),
 .UNSPECIFIED., .F., .F.,
 ( 4, 2, 4 ),
 ( 0.004444412883774334112, 0.006655097293744433734, 0.008865781703714532488 ),
 .UNSPECIFIED. ) ;
#13754 =( LENGTH_UNIT ( ) NAMED_UNIT ( * ) SI_UNIT ( .MILLI., .METRE. ) );
#13755 = CARTESIAN_POINT ( 'NONE',  ( 4.817610911465698642, 0.9367903645274751057, -0.07999226725963382023 ) ) ;
#13756 = AXIS2_PLACEMENT_3D ( 'NONE', #6932, #11677, #9199 ) ;
#13757 = DIRECTION ( 'NONE',  ( -0.000000000000000000, 1.000000000000000000, -0.000000000000000000 ) ) ;
#13758 = CARTESIAN_POINT ( 'NONE',  ( 47.32050807568879947, 0.000000000000000000, -41.96152422706630603 ) ) ;
#13759 = CARTESIAN_POINT ( 'NONE',  ( -4.391654775818395251, 2.390265326283148806, -5.499999997268814944 ) ) ;
#13760 = CARTESIAN_POINT ( 'NONE',  ( 3.061616997868383141E-16, -23.75000000000000000, -5.000000000000000000 ) ) ;
#13761 = EDGE_CURVE ( 'NONE', #10129, #678, #1151, .T. ) ;
#13762 = DIRECTION ( 'NONE',  ( -0.000000000000000000, -0.000000000000000000, 1.000000000000000000 ) ) ;
#13763 = CARTESIAN_POINT ( 'NONE',  ( -34.99999999999999289, -11.00000000000000178, -1.999999999999170441 ) ) ;
#13764 = ORIENTED_EDGE ( 'NONE', *, *, #4546, .F. ) ;
#13765 = DIRECTION ( 'NONE',  ( -1.000000000000000000, 0.000000000000000000, 0.000000000000000000 ) ) ;
#13766 = CARTESIAN_POINT ( 'NONE',  ( 4.276409079477644148, 1.261996585732577891, -8.312499998634407916 ) ) ;
#13767 = FACE_OUTER_BOUND ( 'NONE', #10859, .T. ) ;
#13768 = EDGE_LOOP ( 'NONE', ( #7838, #14736, #9227 ) ) ;
#13769 = ORIENTED_EDGE ( 'NONE', *, *, #14844, .T. ) ;
#13770 = VERTEX_POINT ( 'NONE', #10639 ) ;
#13771 = DIRECTION ( 'NONE',  ( 0.000000000000000000, 1.000000000000000000, 0.000000000000000000 ) ) ;
#13772 = PLANE ( 'NONE',  #3006 ) ;
#13773 = CARTESIAN_POINT ( 'NONE',  ( 42.02221399786069611, -3.000000000000001332, 1.040834085586084257E-13 ) ) ;
#13774 = CARTESIAN_POINT ( 'NONE',  ( -3.280815508853482054, -7.221948645665451139, -7.591546097228400569 ) ) ;
#13775 = CARTESIAN_POINT ( 'NONE',  ( -3.295171437451513974, -7.213553046160526172, -7.590212325761485523 ) ) ;
#13776 = AXIS2_PLACEMENT_3D ( 'NONE', #7265, #5070, #4832 ) ;
#13777 = CARTESIAN_POINT ( 'NONE',  ( -28.86751345948126257, 0.000000000000000000, -18.00000000000001066 ) ) ;
#13778 = CARTESIAN_POINT ( 'NONE',  ( -4.209348295687703967, -3.401574460001763001, -5.437500000000002665 ) ) ;
#13779 = CARTESIAN_POINT ( 'NONE',  ( -45.00000000000000000, -10.00000000000000000, -7.500000000000000000 ) ) ;
#13780 = EDGE_CURVE ( 'NONE', #11117, #4817, #5312, .T. ) ;
#13781 = CARTESIAN_POINT ( 'NONE',  ( 0.000000000000000000, -13.00000000000000178, 0.000000000000000000 ) ) ;
#13782 = ADVANCED_FACE ( 'NONE', ( #4413 ), #15570, .T. ) ;
#13783 = CARTESIAN_POINT ( 'NONE',  ( 2.730187237215162345E-16, -22.18750000136559564, -4.458734124999999437 ) ) ;
#13784 = CARTESIAN_POINT ( 'NONE',  ( 1.261996585732578113, -4.276409079477644148, -7.812499998634407916 ) ) ;
#13785 = ORIENTED_EDGE ( 'NONE', *, *, #671, .T. ) ;
#13786 = DIRECTION ( 'NONE',  ( 0.000000000000000000, 1.000000000000000000, -0.000000000000000000 ) ) ;
#13787 = EDGE_LOOP ( 'NONE', ( #1615, #12335, #6746, #13655, #11977 ) ) ;
#13788 = EDGE_LOOP ( 'NONE', ( #9679, #1697, #15215, #9415, #15856 ) ) ;
#13789 = CARTESIAN_POINT ( 'NONE',  ( 1.846868145590735200, -31.50000000136559564, -4.458734125000000326 ) ) ;
#13790 = CARTESIAN_POINT ( 'NONE',  ( 0.000000000000000000, -20.00000000000000000, 5.000000000000000000 ) ) ;
#13791 = VECTOR ( 'NONE', #7393, 1000.000000000000000 ) ;
#13792 = ORIENTED_EDGE ( 'NONE', *, *, #12699, .T. ) ;
#13793 = CARTESIAN_POINT ( 'NONE',  ( 3.436319922986518449, -2.634841920959471562, -3.531542292954761741 ) ) ;
#13794 = CARTESIAN_POINT ( 'NONE',  ( 11.45098066423670247, -3.000000000000000000, 1.122567565269603304E-11 ) ) ;
#13795 = CARTESIAN_POINT ( 'NONE',  ( -4.276409079477644148, -1.261996585732578335, -0.8124999986344055847 ) ) ;
#13796 = CARTESIAN_POINT ( 'NONE',  ( 21.99999999999956657, -8.786575603324269439E-13, -11.50000000000000000 ) ) ;
#13797 = PRESENTATION_LAYER_ASSIGNMENT (  '', '', ( #13021 ) ) ;
#13798 = CARTESIAN_POINT ( 'NONE',  ( -9.184850993605147944E-16, -28.25000000000000000, 5.000000000000000000 ) ) ;
#13799 = AXIS2_PLACEMENT_3D ( 'NONE', #8431, #8192, #10613 ) ;
#13800 = CARTESIAN_POINT ( 'NONE',  ( -44.05083158856042047, -3.097286126993890942, -21.37039199565628067 ) ) ;
#13801 = CARTESIAN_POINT ( 'NONE',  ( -115.0000000000000142, -10.00000000000000888, -17.50000000000000000 ) ) ;
#13802 = EDGE_CURVE ( 'NONE', #3371, #658, #14198, .T. ) ;
#13803 = CARTESIAN_POINT ( 'NONE',  ( -3.535533905932738641, -29.50000000273118417, 3.535533905932737309 ) ) ;
#13804 = VECTOR ( 'NONE', #9625, 1000.000000000000000 ) ;
#13805 = CARTESIAN_POINT ( 'NONE',  ( -4.795541693661363958, -1.415196051561583790, -3.499999999999999556 ) ) ;
#13806 = CARTESIAN_POINT ( 'NONE',  ( 1.846868145590736310, -30.62500000136559564, 4.458734124999997661 ) ) ;
#13807 = CARTESIAN_POINT ( 'NONE',  ( -44.99999999999999289, -11.00000000000000178, 4.000000000000831335 ) ) ;
#13808 = VERTEX_POINT ( 'NONE', #14020 ) ;
#13809 = ORIENTED_EDGE ( 'NONE', *, *, #15882, .F. ) ;
#13810 = SHAPE_REPRESENTATION_RELATIONSHIP ( 'NONE' , 'NONE' ,  #279, #1156 ) ;
#13811 = VERTEX_POINT ( 'NONE', #10398 ) ;
#13812 = CARTESIAN_POINT ( 'NONE',  ( -44.41643093307008172, -4.472255266399358220, 20.06631602343790632 ) ) ;
#13813 = VECTOR ( 'NONE', #12671, 1000.000000000000000 ) ;
#13814 = ORIENTED_EDGE ( 'NONE', *, *, #7812, .F. ) ;
#13815 = DIRECTION ( 'NONE',  ( -0.5000000000000005551, 0.000000000000000000, 0.8660254037844382635 ) ) ;
#13816 = AXIS2_PLACEMENT_3D ( 'NONE', #7041, #6969, #4449 ) ;
#13817 = VECTOR ( 'NONE', #6864, 1000.000000000000000 ) ;
#13818 =( REPRESENTATION_RELATIONSHIP ('NONE','NONE', #4176, #396 ) REPRESENTATION_RELATIONSHIP_WITH_TRANSFORMATION ( #10297 )SHAPE_REPRESENTATION_RELATIONSHIP( ) );
#13819 = CARTESIAN_POINT ( 'NONE',  ( -3.535533905932737309, -31.62500000000000000, -3.535533905932738197 ) ) ;
#13820 = CARTESIAN_POINT ( 'NONE',  ( 5.000000000000000888, 0.000000000000000000, -25.03750572909317285 ) ) ;
#13821 = FACE_OUTER_BOUND ( 'NONE', #5314, .T. ) ;
#13822 = EDGE_CURVE ( 'NONE', #1389, #4036, #7529, .T. ) ;
#13823 = EDGE_CURVE ( 'NONE', #11644, #1547, #9167, .T. ) ;
#13824 = EDGE_CURVE ( 'NONE', #14832, #10935, #9812, .T. ) ;
#13825 = DIRECTION ( 'NONE',  ( 1.000000000000000000, 6.123233995736766036E-17, -6.123233995736764803E-17 ) ) ;
#13826 = CONICAL_SURFACE ( 'NONE', #10738, 10.39117206796836079, 1.221730476396047926 ) ;
#13827 = CARTESIAN_POINT ( 'NONE',  ( -4.276409079477644148, -1.261996585732578335, -7.062499998634407916 ) ) ;
#13828 = CARTESIAN_POINT ( 'NONE',  ( 5.000000000000004441, 0.000000000000000000, 0.000000000000000000 ) ) ;
#13829 = VERTEX_POINT ( 'NONE', #7163 ) ;
#13830 = CIRCLE ( 'NONE', #12780, 9.999999999999994671 ) ;
#13831 = CARTESIAN_POINT ( 'NONE',  ( 0.000000000000000000, 0.000000000000000000, -25.03750572909317285 ) ) ;
#13832 = CLOSED_SHELL ( 'NONE', ( #12367, #10546, #3810, #15812, #13134, #14134, #14069, #12348, #4031, #8354, #763, #3332, #18, #14272 ) ) ;
#13833 = PRESENTATION_STYLE_ASSIGNMENT (( #4137 ) ) ;
#13834 = EDGE_LOOP ( 'NONE', ( #930, #13976, #306, #5918 ) ) ;
#13835 = CARTESIAN_POINT ( 'NONE',  ( -4.209348295687703079, -3.401574460001763445, -7.437500000000004441 ) ) ;
#13836 = DIRECTION ( 'NONE',  ( -0.000000000000000000, 1.000000000000000000, -0.000000000000000000 ) ) ;
#13837 = ORIENTED_EDGE ( 'NONE', *, *, #12564, .F. ) ;
#13838 = CONTEXT_DEPENDENT_SHAPE_REPRESENTATION ( #6409, #5068 ) ;
#13839 = CARTESIAN_POINT ( 'NONE',  ( 0.5093500532425063732, 4.799145180956616130, -5.374999998634405252 ) ) ;
#13840 = VECTOR ( 'NONE', #9181, 1000.000000000000000 ) ;
#13841 = AXIS2_PLACEMENT_3D ( 'NONE', #7542, #853, #12281 ) ;
#13842 = CARTESIAN_POINT ( 'NONE',  ( 1.415196051561583790, -4.795541693661363958, -5.124999997268817609 ) ) ;
#13843 = CLOSED_SHELL ( 'NONE', ( #10491, #6522, #9171, #8699, #5243, #9251, #8200, #12109, #2130, #1778 ) ) ;
#13844 = FACE_OUTER_BOUND ( 'NONE', #3757, .T. ) ;
#13845 = UNCERTAINTY_MEASURE_WITH_UNIT (LENGTH_MEASURE( 1.000000000000000082E-05 ), #10499, 'distance_accuracy_value', 'NONE');
#13846 = EDGE_CURVE ( 'NONE', #1651, #3972, #2182, .T. ) ;
#13847 = DIRECTION ( 'NONE',  ( 0.000000000000000000, 0.000000000000000000, -1.000000000000000000 ) ) ;
#13848 = CARTESIAN_POINT ( 'NONE',  ( 5.381735091635035495, -0.5711823568785978633, -1.937499997268816276 ) ) ;
#13849 = LINE ( 'NONE', #13928, #101 ) ;
#13850 = AXIS2_PLACEMENT_3D ( 'NONE', #15256, #5704, #4247 ) ;
#13851 = DIRECTION ( 'NONE',  ( 1.000000000000000000, 0.000000000000000000, 0.000000000000000000 ) ) ;
#13852 = DIRECTION ( 'NONE',  ( 1.000000000000000000, 0.000000000000000000, 0.000000000000000000 ) ) ;
#13853 = ORIENTED_EDGE ( 'NONE', *, *, #6935, .F. ) ;
#13854 = FACE_OUTER_BOUND ( 'NONE', #10266, .T. ) ;
#13855 = CARTESIAN_POINT ( 'NONE',  ( 7.500000000000002665, -3.608439182435168036, -7.298562697733106397 ) ) ;
#13856 = CARTESIAN_POINT ( 'NONE',  ( 24.55500000000002103, 3.061616997868384620E-16, -2.500000000000001332 ) ) ;
#13857 = EDGE_LOOP ( 'NONE', ( #14043, #6180, #2962, #11509 ) ) ;
#13858 = ORIENTED_EDGE ( 'NONE', *, *, #3425, .F. ) ;
#13859 = UNCERTAINTY_MEASURE_WITH_UNIT (LENGTH_MEASURE( 1.000000000000000082E-05 ), #13328, 'distance_accuracy_value', 'NONE');
#13860 = ORIENTED_EDGE ( 'NONE', *, *, #1610, .F. ) ;
#13861 = FACE_OUTER_BOUND ( 'NONE', #4304, .T. ) ;
#13862 = PLANE ( 'NONE',  #699 ) ;
#13863 = DIRECTION ( 'NONE',  ( -1.000000000000000000, 0.000000000000000000, 0.000000000000000000 ) ) ;
#13864 = AXIS2_PLACEMENT_3D ( 'NONE', #9279, #9350, #9428 ) ;
#13865 = DIRECTION ( 'NONE',  ( 0.000000000000000000, 0.000000000000000000, -1.000000000000000000 ) ) ;
#13866 = CARTESIAN_POINT ( 'NONE',  ( -3.093533885184382104, -6.874201416485830940, -7.446478553994769989 ) ) ;
#13867 = CARTESIAN_POINT ( 'NONE',  ( 5.000000000000004441, -2.247904837838113790E-16, -6.045263047592945860 ) ) ;
#13868 = AXIS2_PLACEMENT_3D ( 'NONE', #14922, #5292, #10072 ) ;
#13869 = CARTESIAN_POINT ( 'NONE',  ( 2.390265326283148806, 4.391654775818395251, -3.875000000000000000 ) ) ;
#13870 = DIRECTION ( 'NONE',  ( -1.000000000000000000, -0.000000000000000000, -0.000000000000000000 ) ) ;
#13871 = CARTESIAN_POINT ( 'NONE',  ( 19.99999999999956657, -8.786575603324269439E-13, -11.50000000000000000 ) ) ;
#13872 = CARTESIAN_POINT ( 'NONE',  ( 3.152801135295366208, -21.56250000136559208, 3.152801135295367985 ) ) ;
#13873 = CARTESIAN_POINT ( 'NONE',  ( -3.916244202832140253, 2.131511515620587272, -6.187499998634407028 ) ) ;
#13874 = EDGE_LOOP ( 'NONE', ( #11866, #9841, #8842, #7633 ) ) ;
#13875 = CIRCLE ( 'NONE', #5887, 2.649999999999992806 ) ;
#13876 = DIRECTION ( 'NONE',  ( -1.000000000000000000, -0.000000000000000000, -0.000000000000000000 ) ) ;
#13877 = EDGE_LOOP ( 'NONE', ( #9489, #6118, #3421, #12120, #9947 ) ) ;
#13878 = ORIENTED_EDGE ( 'NONE', *, *, #5802, .T. ) ;
#13879 = CARTESIAN_POINT ( 'NONE',  ( 3.152801135295367541, -30.56250000136559564, -3.152801135295367541 ) ) ;
#13880 = DIRECTION ( 'NONE',  ( 0.000000000000000000, 0.000000000000000000, -1.000000000000000000 ) ) ;
#13881 = ORIENTED_EDGE ( 'NONE', *, *, #12912, .T. ) ;
#13882 = AXIS2_PLACEMENT_3D ( 'NONE', #7356, #12182, #12263 ) ;
#13883 = CYLINDRICAL_SURFACE ( 'NONE', #14084, 5.000000000000000888 ) ;
#13884 = EDGE_CURVE ( 'NONE', #3455, #8368, #13194, .T. ) ;
#13885 = EDGE_CURVE ( 'NONE', #6744, #11827, #8399, .T. ) ;
#13887 =( GEOMETRIC_REPRESENTATION_CONTEXT ( 3 ) GLOBAL_UNCERTAINTY_ASSIGNED_CONTEXT ( ( #6613 ) ) GLOBAL_UNIT_ASSIGNED_CONTEXT ( ( #4813, #3598, #12073 ) ) REPRESENTATION_CONTEXT ( 'NONE', 'WORKASPACE' ) );
#13886 = DIRECTION ( 'NONE',  ( 0.000000000000000000, -1.000000000000000000, 0.000000000000000000 ) ) ;
#13888 = CARTESIAN_POINT ( 'NONE',  ( 2.131511515620586383, 3.916244202832140253, -2.187499998634407028 ) ) ;
#13889 = DIRECTION ( 'NONE',  ( 0.000000000000000000, 0.000000000000000000, -1.000000000000000000 ) ) ;
#13890 = VECTOR ( 'NONE', #3413, 1000.000000000000000 ) ;
#13891 = CARTESIAN_POINT ( 'NONE',  ( 3.061616997868383141E-16, -28.75000000000000000, -5.000000000000000000 ) ) ;
#13892 = CARTESIAN_POINT ( 'NONE',  ( -1.393927851585477606, 4.043713361053528743, -3.526374918436835149 ) ) ;
#13893 = CIRCLE ( 'NONE', #14121, 2.649999999999985700 ) ;
#13894 = CARTESIAN_POINT ( 'NONE',  ( 2.500000000000000000, 2.357898499370433054, -1.951563910473907981E-15 ) ) ;
#13895 = CARTESIAN_POINT ( 'NONE',  ( 2.071067811865476394, -26.31250000273118417, 5.000000000000000000 ) ) ;
#13896 = CARTESIAN_POINT ( 'NONE',  ( -43.99999999999978684, -9.000000000000001776, 1.499999999999998668 ) ) ;
#13897 = AXIS2_PLACEMENT_3D ( 'NONE', #15553, #6821, #13103 ) ;
#13898 = CARTESIAN_POINT ( 'NONE',  ( -1.846868145590734756, -27.12500000136559564, -4.458734124999999437 ) ) ;
#13899 = CARTESIAN_POINT ( 'NONE',  ( 5.200000000000002842, 0.000000000000000000, -2.700000000000001066 ) ) ;
#13900 = ORIENTED_EDGE ( 'NONE', *, *, #14393, .T. ) ;
#13901 = VERTEX_POINT ( 'NONE', #12062 ) ;
#13902 = ORIENTED_EDGE ( 'NONE', *, *, #10732, .T. ) ;
#13903 = FACE_OUTER_BOUND ( 'NONE', #424, .T. ) ;
#13904 = AXIS2_PLACEMENT_3D ( 'NONE', #10182, #7442, #2730 ) ;
#13905 = ORIENTED_EDGE ( 'NONE', *, *, #4255, .F. ) ;
#13906 = DIRECTION ( 'NONE',  ( 0.000000000000000000, 0.000000000000000000, 1.000000000000000000 ) ) ;
#13907 = ADVANCED_FACE ( 'NONE', ( #1237 ), #5860, .T. ) ;
#13908 = EDGE_CURVE ( 'NONE', #11317, #15266, #15737, .T. ) ;
#13909 = MANIFOLD_SOLID_BREP ( 'CirPattern3', #11516 ) ;
#13910 = CARTESIAN_POINT ( 'NONE',  ( 7.907996613752301229, 3.055722423191985726, -7.792112796859421486 ) ) ;
#13911 = CARTESIAN_POINT ( 'NONE',  ( -4.458734125000000326, -30.25000000136559564, -1.846868145590735644 ) ) ;
#13912 = CARTESIAN_POINT ( 'NONE',  ( -3.401574460001765221, 4.209348295687701302, -5.687500000000003553 ) ) ;
#13913 = CARTESIAN_POINT ( 'NONE',  ( -0.5093500532425060401, -4.799145180956616130, -3.874999998634408360 ) ) ;
#13914 = FACE_OUTER_BOUND ( 'NONE', #11975, .T. ) ;
#13915 = VERTEX_POINT ( 'NONE', #15880 ) ;
#13916 = CYLINDRICAL_SURFACE ( 'NONE', #741, 5.000000000000000000 ) ;
#13917 = ORIENTED_EDGE ( 'NONE', *, *, #9791, .T. ) ;
#13918 = CARTESIAN_POINT ( 'NONE',  ( -55.00000000000000000, -9.999999999999996447, -17.50000000000000000 ) ) ;
#13919 = CARTESIAN_POINT ( 'NONE',  ( -35.00000000000000000, 37.00000000000000000, 0.000000000000000000 ) ) ;
#13920 = ORIENTED_EDGE ( 'NONE', *, *, #14575, .T. ) ;
#13921 = CARTESIAN_POINT ( 'NONE',  ( -1.261996585732579224, 4.276409079477648589, -6.312499998634407028 ) ) ;
#13922 = EDGE_CURVE ( 'NONE', #621, #5426, #14663, .T. ) ;
#13923 = EDGE_CURVE ( 'NONE', #8374, #8967, #403, .T. ) ;
#13924 = CARTESIAN_POINT ( 'NONE',  ( 4.795541693661363958, 1.415196051561583790, -4.874999997268817609 ) ) ;
#13925 = CARTESIAN_POINT ( 'NONE',  ( 4.631580223510930239, 1.444531747605005878E-11, -0.2579703047231843294 ) ) ;
#13926 = CARTESIAN_POINT ( 'NONE',  ( 0.000000000000000000, -20.00000000000000000, 0.000000000000000000 ) ) ;
#13927 = CARTESIAN_POINT ( 'NONE',  ( -2.390265326283148806, -4.391654775818394363, -2.249999997268815388 ) ) ;
#13928 = CARTESIAN_POINT ( 'NONE',  ( 30.02221399786055755, -20.00000000000000000, -15.99999999999999645 ) ) ;
#13929 = CARTESIAN_POINT ( 'NONE',  ( 6.000000000000000000, -13.00000000000000178, 1.500000000000000000 ) ) ;
#13930 = CARTESIAN_POINT ( 'NONE',  ( 1.846868145590736310, -22.87500000136559564, 4.458734124999997661 ) ) ;
#13931 = ORIENTED_EDGE ( 'NONE', *, *, #13213, .F. ) ;
#13932 = CARTESIAN_POINT ( 'NONE',  ( -41.99999999999978684, -9.000000000000001776, 1.499999999999999112 ) ) ;
#13933 = CARTESIAN_POINT ( 'NONE',  ( -3.753672977998669946, -3.033343224707661712, -6.749999998634408804 ) ) ;
#13934 = ORIENTED_EDGE ( 'NONE', *, *, #14524, .T. ) ;
#13935 = ORIENTED_EDGE ( 'NONE', *, *, #1995, .T. ) ;
#13936 = ORIENTED_EDGE ( 'NONE', *, *, #4893, .F. ) ;
#13937 = DIRECTION ( 'NONE',  ( 0.000000000000000000, 0.000000000000000000, 1.000000000000000000 ) ) ;
#13938 = EDGE_CURVE ( 'NONE', #3489, #3157, #9179, .T. ) ;
#13939 = DIRECTION ( 'NONE',  ( -1.000000000000000000, -0.000000000000000000, -0.000000000000000000 ) ) ;
#13940 = EDGE_CURVE ( 'NONE', #13189, #9048, #4783, .T. ) ;
#13941 = CARTESIAN_POINT ( 'NONE',  ( 2.143131898507869826E-15, 40.00000000000000000, -67.50000000000000000 ) ) ;
#13942 = DIRECTION ( 'NONE',  ( 0.000000000000000000, 0.000000000000000000, 1.000000000000000000 ) ) ;
#13943 = LINE ( 'NONE', #7755, #12959 ) ;
#13944 = PRESENTATION_LAYER_ASSIGNMENT (  '', '', ( #4922 ) ) ;
#13945 = CYLINDRICAL_SURFACE ( 'NONE', #2803, 5.000000000000000000 ) ;
#13946 = CARTESIAN_POINT ( 'NONE',  ( -0.5711823568785978633, -5.381735091635035495, -4.312500000000000000 ) ) ;
#13947 = DIRECTION ( 'NONE',  ( 0.000000000000000000, 0.000000000000000000, 1.000000000000000000 ) ) ;
#13948 = CARTESIAN_POINT ( 'NONE',  ( -0.6810597143197697489, -4.461075778259609770, -3.598441714920717516 ) ) ;
#13949 = CARTESIAN_POINT ( 'NONE',  ( -8.190561711645485556E-16, -21.68750000136559208, 4.458734124999999437 ) ) ;
#13950 = CARTESIAN_POINT ( 'NONE',  ( 1.261996585732578113, -4.276409079477644148, -4.812499998634405252 ) ) ;
#13951 = ORIENTED_EDGE ( 'NONE', *, *, #14643, .F. ) ;
#13952 = CARTESIAN_POINT ( 'NONE',  ( 7.549006887134069643, -4.358421158401204032, -7.700127545397315032 ) ) ;
#13953 = EDGE_LOOP ( 'NONE', ( #13934, #11488, #224, #12949 ) ) ;
#13954 = ORIENTED_EDGE ( 'NONE', *, *, #15710, .T. ) ;
#13955 = ORIENTED_EDGE ( 'NONE', *, *, #6738, .T. ) ;
#13956 = CARTESIAN_POINT ( 'NONE',  ( -3.152801135295367096, -29.31250000136559564, -3.152801135295367541 ) ) ;
#13957 = DIRECTION ( 'NONE',  ( 0.000000000000000000, -1.000000000000000000, 0.000000000000000000 ) ) ;
#13958 = EDGE_CURVE ( 'NONE', #10113, #4642, #2297, .T. ) ;
#13959 = ORIENTED_EDGE ( 'NONE', *, *, #12641, .F. ) ;
#13960 = CARTESIAN_POINT ( 'NONE',  ( -6.765421556309547668E-13, 37.00000000000000000, 67.49999999999930367 ) ) ;
#13961 = CARTESIAN_POINT ( 'NONE',  ( 7.908217798048329250, 3.084840533507072102, -7.795645399445197299 ) ) ;
#13962 = CARTESIAN_POINT ( 'NONE',  ( -3.916244202832140253, 2.131511515620587272, -1.937499998634406584 ) ) ;
#13963 = CARTESIAN_POINT ( 'NONE',  ( -39.99999999999999289, -11.00000000000000178, 8.300651832549021947E-13 ) ) ;
#13964 = CARTESIAN_POINT ( 'NONE',  ( -5.000000000000000888, -30.56250000000000000, -2.071067811865475949 ) ) ;
#13965 = CARTESIAN_POINT ( 'NONE',  ( -4.799145180956616130, 0.5093500532425063732, -3.874999998634404363 ) ) ;
#13966 = CARTESIAN_POINT ( 'NONE',  ( -0.6250000000000003331, -8.299410119600885594, -7.298562697733111726 ) ) ;
#13967 = DIRECTION ( 'NONE',  ( 1.239088197126290570E-16, -0.000000000000000000, 1.000000000000000000 ) ) ;
#13968 = CARTESIAN_POINT ( 'NONE',  ( -2.071067811865478170, -22.43750000273119127, 5.000000000000000000 ) ) ;
#13969 = DIRECTION ( 'NONE',  ( 0.000000000000000000, 0.000000000000000000, -1.000000000000000000 ) ) ;
#13970 = CARTESIAN_POINT ( 'NONE',  ( 1.846868145590735200, -25.25000000136559564, -4.458734124999999437 ) ) ;
#13971 = EDGE_CURVE ( 'NONE', #1411, #6708, #13267, .T. ) ;
#13972 = CARTESIAN_POINT ( 'NONE',  ( 2.325424218456833003, -7.317669739338271917, -7.030005583190793494 ) ) ;
#13973 = VERTEX_POINT ( 'NONE', #13426 ) ;
#13974 = VERTEX_POINT ( 'NONE', #2367 ) ;
#13975 = PRODUCT_DEFINITION_SHAPE ( 'NONE', 'NONE',  #16000 ) ;
#13976 = ORIENTED_EDGE ( 'NONE', *, *, #14448, .T. ) ;
#13977 = DIRECTION ( 'NONE',  ( 0.000000000000000000, 0.000000000000000000, 1.000000000000000000 ) ) ;
#13978 = VECTOR ( 'NONE', #3502, 1000.000000000000114 ) ;
#13979 = ORIENTED_EDGE ( 'NONE', *, *, #991, .T. ) ;
#13980 = DIRECTION ( 'NONE',  ( -0.000000000000000000, 0.000000000000000000, 1.000000000000000000 ) ) ;
#13981 = CARTESIAN_POINT ( 'NONE',  ( -4.999999999999849898, 1.272547481429008309, -1.461597479913463005 ) ) ;
#13982 = B_SPLINE_CURVE_WITH_KNOTS ( 'NONE', 3,
 ( #7754, #8794, #146, #1585, #13774, #6523, #3926, #5224, #11439, #14847 ),
 .UNSPECIFIED., .F., .F.,
 ( 4, 2, 2, 2, 4 ),
 ( 0.000000000000000000, 0.002305503304226489900, 0.004611006608452982401, 0.006916509912679474036, 0.009222013216905966537 ),
 .UNSPECIFIED. ) ;
#13983 = CARTESIAN_POINT ( 'NONE',  ( -1.846868145590737420, -31.00000000136559564, 4.458734124999999437 ) ) ;
#13984 = CARTESIAN_POINT ( 'NONE',  ( 5.000000000000095923, 0.7223674278660565662, -6.021799365517157554 ) ) ;
#13985 =( BOUNDED_CURVE ( )  B_SPLINE_CURVE ( 2, ( #15865, #3726, #4785, #8670, #5925, #14647, #15221, #6563, #2590, #7543, #13736 ),
 .UNSPECIFIED., .F., .F. ) 
 B_SPLINE_CURVE_WITH_KNOTS ( ( 3, 2, 2, 2, 2, 3 ),
 ( 0.5045872658012773293, 0.5124999999999999556, 0.5250000000000000222, 0.5374999999999999778, 0.5500000000000000444, 0.5545872658012773737 ),
 .UNSPECIFIED. ) 
 CURVE ( )  GEOMETRIC_REPRESENTATION_ITEM ( )  RATIONAL_B_SPLINE_CURVE ( ( 0.9646335149384803742, 0.9518143178943441196, 1.000000000000000000, 0.9238795325112867385, 1.000000000000000000, 0.9238795325112867385, 1.000000000000000000, 0.9238795325112867385, 1.000000000000000000, 0.9720652146169423968, 0.9646335149384803742 ) ) 
 REPRESENTATION_ITEM ( '' )  );
#13986 = CARTESIAN_POINT ( 'NONE',  ( -4.197393957002303999, -7.773935952363655451E-14, -3.503767560748929810 ) ) ;
#13987 = CARTESIAN_POINT ( 'NONE',  ( -0.5093500532425060401, -4.799145180956616130, 1.125000001365592306 ) ) ;
#13988 = EDGE_CURVE ( 'NONE', #15272, #14655, #2699, .T. ) ;
#13990 = EDGE_CURVE ( 'NONE', #6220, #560, #3742, .T. ) ;
#13989 = ORIENTED_EDGE ( 'NONE', *, *, #1971, .F. ) ;
#13991 = SURFACE_SIDE_STYLE ('',( #12768 ) ) ;
#13992 = ORIENTED_EDGE ( 'NONE', *, *, #12980, .T. ) ;
#13993 = CARTESIAN_POINT ( 'NONE',  ( -5.000000000000091482, -0.7223674278660691117, -1.521799365517154667 ) ) ;
#13994 = LINE ( 'NONE', #9011, #3527 ) ;
#13995 = ORIENTED_EDGE ( 'NONE', *, *, #534, .T. ) ;
#13996 = AXIS2_PLACEMENT_3D ( 'NONE', #15126, #4045, #12680 ) ;
#13997 = DIRECTION ( 'NONE',  ( -1.000000000000000000, 0.000000000000000000, 0.000000000000000000 ) ) ;
#13998 = AXIS2_PLACEMENT_3D ( 'NONE', #9999, #7668, #5393 ) ;
#13999 = CARTESIAN_POINT ( 'NONE',  ( 4.391654775818395251, -2.390265326283149694, -4.999999997268817609 ) ) ;
#14000 = CARTESIAN_POINT ( 'NONE',  ( -4.795541693661363958, -1.415196051561583790, -8.374999997268814056 ) ) ;
#14001 = PRODUCT_DEFINITION_CONTEXT ( 'detailed design', #14352, 'design' ) ;
#14003 = CONICAL_SURFACE ( 'NONE', #7058, 5.560781378645573980, 1.221730476396046816 ) ;
#14002 = CARTESIAN_POINT ( 'NONE',  ( 1.415196051561583790, -4.795541693661363958, -7.124999997268815832 ) ) ;
#14004 = CARTESIAN_POINT ( 'NONE',  ( -6.259644161404860030E-16, -4.618802153517027165, -3.433295621305388234 ) ) ;
#14005 = EDGE_CURVE ( 'NONE', #2401, #9162, #1382, .T. ) ;
#14006 = CARTESIAN_POINT ( 'NONE',  ( -4.197393957002303999, -7.773935952363655451E-14, -3.503767560748929810 ) ) ;
#14007 = CARTESIAN_POINT ( 'NONE',  ( 79.38739406438118351, 0.000000000000000000, 12.50099999999964417 ) ) ;
#14008 = ADVANCED_FACE ( 'NONE', ( #13676 ), #7479, .T. ) ;
#14009 = ORIENTED_EDGE ( 'NONE', *, *, #7999, .F. ) ;
#14010 = CARTESIAN_POINT ( 'NONE',  ( 2.500000000000000000, -2.357898499370432610, 3.252606517456513302E-15 ) ) ;
#14011 = CARTESIAN_POINT ( 'NONE',  ( -2.131511515620587272, -3.916244202832140253, -6.687499998634407028 ) ) ;
#14012 = VECTOR ( 'NONE', #12431, 1000.000000000000000 ) ;
#14013 = CARTESIAN_POINT ( 'NONE',  ( -2.071067811865463959, -26.43750000273118772, 5.000000000000013323 ) ) ;
#14014 = EDGE_LOOP ( 'NONE', ( #1372, #8910, #12757, #5807, #7368, #4676 ) ) ;
#14015 = CARTESIAN_POINT ( 'NONE',  ( -45.00000000000000000, 0.000000000000000000, 17.50000000000000000 ) ) ;
#14016 = ORIENTED_EDGE ( 'NONE', *, *, #10103, .F. ) ;
#14017 = VERTEX_POINT ( 'NONE', #1565 ) ;
#14018 = DIRECTION ( 'NONE',  ( -0.000000000000000000, 1.000000000000000000, -0.000000000000000000 ) ) ;
#14019 = DIRECTION ( 'NONE',  ( -0.000000000000000000, 1.000000000000000000, -0.000000000000000000 ) ) ;
#14020 = CARTESIAN_POINT ( 'NONE',  ( -67.50000000000000000, 40.00000000000000000, -2.650000000000699352 ) ) ;
#14021 = VECTOR ( 'NONE', #15655, 1000.000000000000114 ) ;
#14022 = CARTESIAN_POINT ( 'NONE',  ( -28.86751345948126612, -37.00000000000000711, -20.00000000000000355 ) ) ;
#14023 = DIRECTION ( 'NONE',  ( -0.000000000000000000, -0.000000000000000000, -1.000000000000000000 ) ) ;
#14024 = CARTESIAN_POINT ( 'NONE',  ( -7.703920929261759198, -4.447860822324870789, -7.917989418073290153 ) ) ;
#14025 = CARTESIAN_POINT ( 'NONE',  ( 0.5711823568785989735, 5.381735091635026613, -4.812500000000000000 ) ) ;
#14026 = LINE ( 'NONE', #9044, #9624 ) ;
#14027 = EDGE_CURVE ( 'NONE', #13323, #2517, #12382, .T. ) ;
#14028 = DIRECTION ( 'NONE',  ( 1.000000000000000000, -0.000000000000000000, 1.114413700119375779E-16 ) ) ;
#14029 = ADVANCED_FACE ( 'NONE', ( #4957 ), #6503, .F. ) ;
#14030 = CARTESIAN_POINT ( 'NONE',  ( -8.190561711645485556E-16, -24.68750000136559564, 4.458734124999999437 ) ) ;
#14031 = ADVANCED_FACE ( 'NONE', ( #1638 ), #1317, .F. ) ;
#14032 = CARTESIAN_POINT ( 'NONE',  ( -1.261996585732579224, 4.276409079477648589, -8.312499998634407916 ) ) ;
#14033 = ORIENTED_EDGE ( 'NONE', *, *, #10447, .F. ) ;
#14034 = UNCERTAINTY_MEASURE_WITH_UNIT (LENGTH_MEASURE( 1.000000000000000082E-05 ), #2199, 'distance_accuracy_value', 'NONE');
#14035 = FACE_OUTER_BOUND ( 'NONE', #12441, .T. ) ;
#14036 = EDGE_LOOP ( 'NONE', ( #6995, #11702, #454, #4426 ) ) ;
#14037 = VERTEX_POINT ( 'NONE', #8772 ) ;
#14038 = B_SPLINE_CURVE_WITH_KNOTS ( 'NONE', 3,
 ( #6163, #13409, #4699, #14884, #9622, #13480 ),
 .UNSPECIFIED., .F., .F.,
 ( 4, 2, 4 ),
 ( 0.002365888236227995517, 0.003551327329835084114, 0.004736766423442172712 ),
 .UNSPECIFIED. ) ;
#14039 = VERTEX_POINT ( 'NONE', #10136 ) ;
#14040 = CARTESIAN_POINT ( 'NONE',  ( 4.458734124999999437, -30.68750000136559564, 0.000000000000000000 ) ) ;
#14041 = CARTESIAN_POINT ( 'NONE',  ( 9.999999999999891642, -13.00000000000000178, -19.82050807568883499 ) ) ;
#14042 = MANIFOLD_SOLID_BREP ( 'Hex', #15917 ) ;
#14043 = ORIENTED_EDGE ( 'NONE', *, *, #3664, .T. ) ;
#14044 = CARTESIAN_POINT ( 'NONE',  ( 2.807080416178989513, -3.225969019225150003, -3.502507215260505014 ) ) ;
#14045 = AXIS2_PLACEMENT_3D ( 'NONE', #9529, #3145, #8330 ) ;
#14046 = CARTESIAN_POINT ( 'NONE',  ( 7.922811941611899833, 4.628808333142396592, -8.057670691780701944 ) ) ;
#14047 = CARTESIAN_POINT ( 'NONE',  ( 1.261996585732578113, -4.276409079477644148, -5.562499998634406140 ) ) ;
#14048 = FACE_OUTER_BOUND ( 'NONE', #7676, .T. ) ;
#14049 = CARTESIAN_POINT ( 'NONE',  ( -3.535533905932737309, -27.62500000000000000, -3.535533905932738197 ) ) ;
#14050 = CARTESIAN_POINT ( 'NONE',  ( 2.131511515620586383, 3.916244202832140253, -2.187499998634407028 ) ) ;
#14051 = CARTESIAN_POINT ( 'NONE',  ( 10.39117206796836079, 0.000000000000000000, -8.499999999999996447 ) ) ;
#14052 = CARTESIAN_POINT ( 'NONE',  ( 0.000000000000000000, -13.00000000000000178, 0.000000000000000000 ) ) ;
#14053 = CARTESIAN_POINT ( 'NONE',  ( -3.535533905932738641, -23.50000000273118772, 3.535533905932737309 ) ) ;
#14054 = EDGE_CURVE ( 'NONE', #9435, #11992, #2606, .T. ) ;
#14055 = DIRECTION ( 'NONE',  ( -1.734723475976807489E-15, 0.000000000000000000, 1.000000000000000000 ) ) ;
#14056 = AXIS2_PLACEMENT_3D ( 'NONE', #11012, #7065, #5928 ) ;
#14057 = CARTESIAN_POINT ( 'NONE',  ( -4.458734125000000326, -24.87500000136559564, 1.846868145590734089 ) ) ;
#14058 = CARTESIAN_POINT ( 'NONE',  ( 4.795541693661363958, 1.415196051561583790, -7.000000000000002665 ) ) ;
#14059 = ORIENTED_EDGE ( 'NONE', *, *, #888, .F. ) ;
#14060 = EDGE_LOOP ( 'NONE', ( #9657, #13902, #13453, #15959 ) ) ;
#14062 = DIRECTION ( 'NONE',  ( 0.000000000000000000, 0.000000000000000000, 1.000000000000000000 ) ) ;
#14061 = CIRCLE ( 'NONE', #6326, 0.2000000000000000944 ) ;
#14063 = EDGE_LOOP ( 'NONE', ( #14493, #13935, #1314, #3495 ) ) ;
#14064 = DIRECTION ( 'NONE',  ( -1.114413700119375779E-16, 0.000000000000000000, 1.000000000000000000 ) ) ;
#14065 = ORIENTED_EDGE ( 'NONE', *, *, #15753, .T. ) ;
#14066 = DIRECTION ( 'NONE',  ( -0.000000000000000000, -1.000000000000000000, -0.000000000000000000 ) ) ;
#14067 = AXIS2_PLACEMENT_3D ( 'NONE', #7816, #5459, #11430 ) ;
#14068 = AXIS2_PLACEMENT_3D ( 'NONE', #14336, #15855, #8050 ) ;
#14069 = ADVANCED_FACE ( 'NONE', ( #4065 ), #3256, .T. ) ;
#14070 = CARTESIAN_POINT ( 'NONE',  ( 4.795541693661363958, 1.415196051561583790, -1.874999997268814944 ) ) ;
#14071 = AXIS2_PLACEMENT_3D ( 'NONE', #13250, #8440, #2039 ) ;
#14072 = CARTESIAN_POINT ( 'NONE',  ( -8.190561711645485556E-16, -26.93750000136559564, 4.458734124999999437 ) ) ;
#14073 = CARTESIAN_POINT ( 'NONE',  ( 30.02221399786053624, 1.999999999999998224, 16.00000000000001421 ) ) ;
#14074 = CONTEXT_DEPENDENT_SHAPE_REPRESENTATION ( #15709, #14684 ) ;
#14075 = CARTESIAN_POINT ( 'NONE',  ( 5.000000000000095923, 0.7223674278660565662, -7.896799362785968945 ) ) ;
#14076 = LINE ( 'NONE', #1947, #4037 ) ;
#14077 = ORIENTED_EDGE ( 'NONE', *, *, #7809, .F. ) ;
#14078 = ADVANCED_BREP_SHAPE_REPRESENTATION ( '', ( #14732, #3223 ), #5546 ) ;
#14079 = STYLED_ITEM ( 'NONE', ( #178 ), #14760 ) ;
#14080 = EDGE_LOOP ( 'NONE', ( #12732, #10009, #7855, #8708, #10169, #14659, #12473 ) ) ;
#14081 = FACE_OUTER_BOUND ( 'NONE', #14251, .T. ) ;
#14082 = CARTESIAN_POINT ( 'NONE',  ( -4.458734124999999437, -27.93750000136559564, -5.460374474430324690E-16 ) ) ;
#14083 = ORIENTED_EDGE ( 'NONE', *, *, #1181, .T. ) ;
#14084 = AXIS2_PLACEMENT_3D ( 'NONE', #2892, #1680, #4107 ) ;
#14085 = EDGE_CURVE ( 'NONE', #15535, #2621, #7961, .T. ) ;
#14086 = CONTEXT_DEPENDENT_SHAPE_REPRESENTATION ( #10228, #7670 ) ;
#14087 = SURFACE_STYLE_USAGE ( .BOTH. , #9402 ) ;
#14088 = EDGE_CURVE ( 'NONE', #15165, #11995, #8203, .T. ) ;
#14089 = EDGE_CURVE ( 'NONE', #15535, #3133, #2968, .T. ) ;
#14090 =( BOUNDED_CURVE ( )  B_SPLINE_CURVE ( 3, ( #4085, #15008, #11361, #5221 ),
 .UNSPECIFIED., .F., .F. ) 
 B_SPLINE_CURVE_WITH_KNOTS ( ( 4, 4 ),
 ( 0.000000000000000000, 1.570796326794896558 ),
 .UNSPECIFIED. ) 
 CURVE ( )  GEOMETRIC_REPRESENTATION_ITEM ( )  RATIONAL_B_SPLINE_CURVE ( ( 1.000000000000000000, 0.8047378541243649375, 0.8047378541243649375, 1.000000000000000000 ) ) 
 REPRESENTATION_ITEM ( '' )  );
#14091 = AXIS2_PLACEMENT_3D ( 'NONE', #5145, #14925, #9739 ) ;
#14092 = DIRECTION ( 'NONE',  ( 0.000000000000000000, 0.000000000000000000, -1.000000000000000000 ) ) ;
#14093 = DIRECTION ( 'NONE',  ( 0.000000000000000000, 1.000000000000000000, 0.000000000000000000 ) ) ;
#14094 = AXIS2_PLACEMENT_3D ( 'NONE', #13636, #2726, #11217 ) ;
#14095 = CARTESIAN_POINT ( 'NONE',  ( -1.415196051561583790, 4.795541693661363958, -7.624999997268816720 ) ) ;
#14096 = CARTESIAN_POINT ( 'NONE',  ( -124.9999999999999716, -10.00000000000001066, 17.50000000000000000 ) ) ;
#14097 = MANIFOLD_SOLID_BREP ( 'Hex', #189 ) ;
#14098 = DIRECTION ( 'NONE',  ( -1.000000000000000000, -0.000000000000000000, -0.000000000000000000 ) ) ;
#14099 = CARTESIAN_POINT ( 'NONE',  ( -3.152801135295367096, -22.31250000136559564, -3.152801135295367541 ) ) ;
#14100 = VERTEX_POINT ( 'NONE', #1958 ) ;
#14101 = CARTESIAN_POINT ( 'NONE',  ( 4.504907258964289340, -0.3910024795134889319, -0.3378236062164368114 ) ) ;
#14102 = DIRECTION ( 'NONE',  ( -1.000000000000000000, -0.000000000000000000, -0.000000000000000000 ) ) ;
#14103 = CARTESIAN_POINT ( 'NONE',  ( 6.902527771671632451, 4.675077770780897701, -0.7026937717022812002 ) ) ;
#14104 = ORIENTED_EDGE ( 'NONE', *, *, #11570, .F. ) ;
#14105 = AXIS2_PLACEMENT_3D ( 'NONE', #14652, #5931, #2356 ) ;
#14106 = ORIENTED_EDGE ( 'NONE', *, *, #13195, .T. ) ;
#14107 = ORIENTED_EDGE ( 'NONE', *, *, #4867, .F. ) ;
#14108 = DIRECTION ( 'NONE',  ( -0.000000000000000000, 1.000000000000000000, -0.000000000000000000 ) ) ;
#14109 = CARTESIAN_POINT ( 'NONE',  ( -4.175648173966055587, 2.207990556236529844, -3.469390959564062626 ) ) ;
#14110 = AXIS2_PLACEMENT_3D ( 'NONE', #1508, #13695, #12561 ) ;
#14111 = DIRECTION ( 'NONE',  ( 0.000000000000000000, 1.000000000000000000, 0.000000000000000000 ) ) ;
#14112 = EDGE_CURVE ( 'NONE', #3896, #15071, #442, .T. ) ;
#14113 = CARTESIAN_POINT ( 'NONE',  ( -9.184850993605147944E-16, -25.37500000273118417, 5.000000000000000000 ) ) ;
#14115 = FACE_OUTER_BOUND ( 'NONE', #10669, .T. ) ;
#14114 = AXIS2_PLACEMENT_3D ( 'NONE', #14602, #9524, #8324 ) ;
#14116 = CARTESIAN_POINT ( 'NONE',  ( -7.922281120364393914, -4.573931137438277617, -8.047472243342932430 ) ) ;
#14117 = FACE_OUTER_BOUND ( 'NONE', #891, .T. ) ;
#14118 = LINE ( 'NONE', #7991, #8229 ) ;
#14119 = DIRECTION ( 'NONE',  ( 0.8660254037844384856, -0.000000000000000000, 0.5000000000000004441 ) ) ;
#14120 = CARTESIAN_POINT ( 'NONE',  ( -44.99999999999999289, -13.00000000000000178, -3.999999999999170885 ) ) ;
#14121 = AXIS2_PLACEMENT_3D ( 'NONE', #15811, #3748, #13599 ) ;
#14122 = CIRCLE ( 'NONE', #11278, 2.649999999999985700 ) ;
#14123 = CARTESIAN_POINT ( 'NONE',  ( -3.753672977998669946, -3.033343224707661712, -4.999999998634407028 ) ) ;
#14124 = EDGE_LOOP ( 'NONE', ( #14409, #4238, #4677, #5567 ) ) ;
#14125 = DIRECTION ( 'NONE',  ( 0.000000000000000000, 0.000000000000000000, 1.000000000000000000 ) ) ;
#14126 = ORIENTED_EDGE ( 'NONE', *, *, #7190, .T. ) ;
#14127 = ORIENTED_EDGE ( 'NONE', *, *, #15197, .F. ) ;
#14128 = PRESENTATION_STYLE_ASSIGNMENT (( #15431 ) ) ;
#14129 = CARTESIAN_POINT ( 'NONE',  ( 4.458734124999999437, -30.75000000136559564, 1.846868145590737864 ) ) ;
#14130 = CARTESIAN_POINT ( 'NONE',  ( -91.33974596215558961, -105.7735026918962404, -7.500000000000001776 ) ) ;
#14131 = AXIS2_PLACEMENT_3D ( 'NONE', #1748, #7905, #6695 ) ;
#14132 = ORIENTED_EDGE ( 'NONE', *, *, #12398, .F. ) ;
#14133 = DIRECTION ( 'NONE',  ( -1.000000000000000000, -0.000000000000000000, -0.000000000000000000 ) ) ;
#14134 = ADVANCED_FACE ( 'NONE', ( #10308 ), #6668, .F. ) ;
#14135 = EDGE_CURVE ( 'NONE', #5622, #1601, #14326, .T. ) ;
#14136 = CARTESIAN_POINT ( 'NONE',  ( 0.000000000000000000, 0.000000000000000000, -25.03750572909317285 ) ) ;
#14137 = CARTESIAN_POINT ( 'NONE',  ( 3.916244202832140253, -2.131511515620588160, -5.437499998634406140 ) ) ;
#14138 = CARTESIAN_POINT ( 'NONE',  ( -3.401574460001765221, 4.209348295687701302, -5.562499997268814056 ) ) ;
#14139 = CARTESIAN_POINT ( 'NONE',  ( 5.000000000000000888, -24.93750000000000355, -2.071067811865475505 ) ) ;
#14140 = CARTESIAN_POINT ( 'NONE',  ( -1.415196051561583790, 4.795541693661363958, 1.249999999999997558 ) ) ;
#14141 = CARTESIAN_POINT ( 'NONE',  ( -44.24585618745123128, -3.477892933143074572, -20.69602687709009459 ) ) ;
#14142 = AXIS2_PLACEMENT_3D ( 'NONE', #14476, #8346, #2180 ) ;
#14143 = CARTESIAN_POINT ( 'NONE',  ( 0.000000000000000000, 40.00000000000000000, 0.000000000000000000 ) ) ;
#14144 = CARTESIAN_POINT ( 'NONE',  ( 5.000000000000000000, -25.12500000273118417, 0.000000000000000000 ) ) ;
#14145 = AXIS2_PLACEMENT_3D ( 'NONE', #5516, #5440, #13009 ) ;
#14146 = ORIENTED_EDGE ( 'NONE', *, *, #11371, .T. ) ;
#14147 = CARTESIAN_POINT ( 'NONE',  ( -3.152801135295367096, -28.06250000136559564, -3.152801135295367541 ) ) ;
#14148 = CARTESIAN_POINT ( 'NONE',  ( 9.999999999999891642, -13.00000000000000178, -19.82050807568883499 ) ) ;
#14149 = ORIENTED_EDGE ( 'NONE', *, *, #7687, .T. ) ;
#14150 = ORIENTED_EDGE ( 'NONE', *, *, #4049, .F. ) ;
#14151 = CARTESIAN_POINT ( 'NONE',  ( -7.500000000000003553, 4.730921838224047882, -7.493596905200506697 ) ) ;
#14152 = AXIS2_PLACEMENT_3D ( 'NONE', #825, #15780, #8432 ) ;
#14153 = ORIENTED_EDGE ( 'NONE', *, *, #316, .F. ) ;
#14154 = DIRECTION ( 'NONE',  ( 0.000000000000000000, 0.000000000000000000, 1.000000000000000000 ) ) ;
#14155 = B_SPLINE_CURVE_WITH_KNOTS ( 'NONE', 3,
 ( #496, #10352, #6473, #12591, #10105, #11385, #4193, #13966, #7848 ),
 .UNSPECIFIED., .F., .F.,
 ( 4, 2, 1, 2, 4 ),
 ( 0.000000000000000000, 0.002165063509461097931, 0.004330127018922195863, 0.006495190528383293360, 0.008660254037844391725 ),
 .UNSPECIFIED. ) ;
#14156 = ORIENTED_EDGE ( 'NONE', *, *, #499, .T. ) ;
#14157 = FACE_OUTER_BOUND ( 'NONE', #4882, .T. ) ;
#14158 = AXIS2_PLACEMENT_3D ( 'NONE', #12486, #6373, #1519 ) ;
#14159 = AXIS2_PLACEMENT_3D ( 'NONE', #5454, #613, #1806 ) ;
#14160 = EDGE_CURVE ( 'NONE', #5937, #2247, #12941, .T. ) ;
#14161 = PRODUCT_DEFINITION_SHAPE ( 'NONE', 'NONE',  #15968 ) ;
#14162 = CARTESIAN_POINT ( 'NONE',  ( -5.000000000000000888, -31.43750000000000000, 2.071067811865474617 ) ) ;
#14163 = CARTESIAN_POINT ( 'NONE',  ( -4.458734124999999437, -29.18750000136559564, -5.460374474430324690E-16 ) ) ;
#14164 = VECTOR ( 'NONE', #3730, 1000.000000000000114 ) ;
#14165 = CARTESIAN_POINT ( 'NONE',  ( -9.184850993605147944E-16, -24.25000000000000000, 5.000000000000000000 ) ) ;
#14166 = DIRECTION ( 'NONE',  ( 1.000000000000000000, 0.000000000000000000, 0.000000000000000000 ) ) ;
#14167 = APPLICATION_PROTOCOL_DEFINITION ( 'draft international standard', 'automotive_design', 1998, #1125 ) ;
#14168 = CARTESIAN_POINT ( 'NONE',  ( -5.000000000000002665, -1.404940523648820476E-14, -7.420263044861759028 ) ) ;
#14169 = CARTESIAN_POINT ( 'NONE',  ( -4.276409079477644148, -1.261996585732578335, 0.9375000013655925279 ) ) ;
#14170 = VECTOR ( 'NONE', #3329, 1000.000000000000000 ) ;
#14171 = EDGE_LOOP ( 'NONE', ( #7513, #8178, #6219, #3273, #15004, #15264, #12838, #15559, #6217, #11090, #11867, #7057, #6706, #12613, #1891, #2921, #7328, #8116, #3866, #6385, #14104, #2437 ) ) ;
#14172 = VECTOR ( 'NONE', #11705, 1000.000000000000000 ) ;
#14173 = ORIENTED_EDGE ( 'NONE', *, *, #1622, .T. ) ;
#14174 = CARTESIAN_POINT ( 'NONE',  ( -7.970070017554224506, 4.546953124339779606, -8.057670357645367432 ) ) ;
#14175 = AXIS2_PLACEMENT_3D ( 'NONE', #9729, #121, #7244 ) ;
#14176 = ORIENTED_EDGE ( 'NONE', *, *, #475, .T. ) ;
#14177 = VERTEX_POINT ( 'NONE', #1719 ) ;
#14178 = AXIS2_PLACEMENT_3D ( 'NONE', #10028, #7695, #10187 ) ;
#14179 = VECTOR ( 'NONE', #3867, 1000.000000000000000 ) ;
#14180 = CARTESIAN_POINT ( 'NONE',  ( 2.143131898507869826E-15, 40.00000000000000000, -70.15000000000000568 ) ) ;
#14181 = DIRECTION ( 'NONE',  ( -0.000000000000000000, -1.000000000000000000, -0.000000000000000000 ) ) ;
#14182 = CARTESIAN_POINT ( 'NONE',  ( 2.390265326283148806, 4.391654775818395251, -7.749999997268816720 ) ) ;
#14183 = CARTESIAN_POINT ( 'NONE',  ( -41.99999999999978684, -9.000000000000001776, 3.499999999999998668 ) ) ;
#14184 = CARTESIAN_POINT ( 'NONE',  ( 2.390265326283148806, 4.391654775818395251, -1.875000000000001776 ) ) ;
#14185 = LINE ( 'NONE', #6070, #6334 ) ;
#14186 = ORIENTED_EDGE ( 'NONE', *, *, #11988, .T. ) ;
#14187 = DIRECTION ( 'NONE',  ( 1.000000000000000000, 0.000000000000000000, 3.343241100358131282E-16 ) ) ;
#14188 = CARTESIAN_POINT ( 'NONE',  ( -90.00000000000000000, -95.00000000000000000, -7.500000000000000000 ) ) ;
#14189 = FILL_AREA_STYLE ('',( #12055 ) ) ;
#14190 = EDGE_CURVE ( 'NONE', #8804, #9361, #12239, .T. ) ;
#14191 = ORIENTED_EDGE ( 'NONE', *, *, #11555, .T. ) ;
#14192 = DIRECTION ( 'NONE',  ( -0.4999999999999997224, 0.000000000000000000, -0.8660254037844388186 ) ) ;
#14193 = VERTEX_POINT ( 'NONE', #6820 ) ;
#14194 = ORIENTED_EDGE ( 'NONE', *, *, #7044, .T. ) ;
#14195 = CARTESIAN_POINT ( 'NONE',  ( 2.071067811865461294, -22.93750000273118417, -5.000000000000014211 ) ) ;
#14196 = DIRECTION ( 'NONE',  ( 0.000000000000000000, 0.000000000000000000, 1.000000000000000000 ) ) ;
#14197 =( BOUNDED_CURVE ( )  B_SPLINE_CURVE ( 3, ( #8031, #1858, #665, #12029 ),
 .UNSPECIFIED., .F., .F. ) 
 B_SPLINE_CURVE_WITH_KNOTS ( ( 4, 4 ),
 ( 3.141592653589793116, 4.712388980384691450 ),
 .UNSPECIFIED. ) 
 CURVE ( )  GEOMETRIC_REPRESENTATION_ITEM ( )  RATIONAL_B_SPLINE_CURVE ( ( 1.000000000000000000, 0.8047378541243646044, 0.8047378541243646044, 1.000000000000000000 ) ) 
 REPRESENTATION_ITEM ( '' )  );
#14198 = LINE ( 'NONE', #3195, #6067 ) ;
#14199 = CARTESIAN_POINT ( 'NONE',  ( -41.99999999999978684, -9.000000000000001776, -3.500000000000000888 ) ) ;
#14200 = CARTESIAN_POINT ( 'NONE',  ( -2.071067811865460850, -25.68750000000000355, -5.000000000000014211 ) ) ;
#14201 = DIRECTION ( 'NONE',  ( 0.000000000000000000, 1.000000000000000000, 0.000000000000000000 ) ) ;
#14202 = CARTESIAN_POINT ( 'NONE',  ( -1.415196051561583790, 4.795541693661363958, -7.750000000000003553 ) ) ;
#14203 = CARTESIAN_POINT ( 'NONE',  ( 4.769696007084728073, -13.00000000000000178, 1.500000000000000000 ) ) ;
#14204 = DIRECTION ( 'NONE',  ( 0.000000000000000000, -1.000000000000000000, 0.000000000000000000 ) ) ;
#14205 = CARTESIAN_POINT ( 'NONE',  ( 4.458734124999999437, -29.68750000136559208, 0.000000000000000000 ) ) ;
#14206 = CARTESIAN_POINT ( 'NONE',  ( -3.033343224707664376, 3.753672977998667726, 1.000000001365594082 ) ) ;
#14207 = ORIENTED_EDGE ( 'NONE', *, *, #5298, .F. ) ;
#14208 = CARTESIAN_POINT ( 'NONE',  ( -36.99999999999999289, -11.00000000000000178, 4.000000000000832223 ) ) ;
#14209 = EDGE_CURVE ( 'NONE', #15920, #2123, #11808, .T. ) ;
#14210 = B_SPLINE_CURVE_WITH_KNOTS ( 'NONE', 3,
 ( #1900, #14275, #4491, #4571, #14437, #14583 ),
 .UNSPECIFIED., .F., .F.,
 ( 4, 2, 4 ),
 ( 0.003358874760055551890, 0.004541967308452098118, 0.005725059856848645212 ),
 .UNSPECIFIED. ) ;
#14211 = ORIENTED_EDGE ( 'NONE', *, *, #3443, .F. ) ;
#14212 = ORIENTED_EDGE ( 'NONE', *, *, #2887, .F. ) ;
#14213 = EDGE_CURVE ( 'NONE', #739, #13011, #8120, .T. ) ;
#14214 =( LENGTH_UNIT ( ) NAMED_UNIT ( * ) SI_UNIT ( .MILLI., .METRE. ) );
#14215 = CARTESIAN_POINT ( 'NONE',  ( -3.152801135295367985, -29.06250000136559564, 3.152801135295367096 ) ) ;
#14216 = DIRECTION ( 'NONE',  ( 0.000000000000000000, -1.000000000000000000, 1.287488025362403787E-15 ) ) ;
#14217 = ORIENTED_EDGE ( 'NONE', *, *, #10156, .F. ) ;
#14218 = CARTESIAN_POINT ( 'NONE',  ( -2.071067811865478170, -28.31250000000000000, 5.000000000000000000 ) ) ;
#14219 = DIRECTION ( 'NONE',  ( 0.000000000000000000, 1.000000000000000000, -1.224646799147353207E-16 ) ) ;
#14220 = CARTESIAN_POINT ( 'NONE',  ( 3.033343224707661712, -3.753672977998669502, -6.499999998634408804 ) ) ;
#14221 = CARTESIAN_POINT ( 'NONE',  ( -34.99999999999999289, -11.00000000000000178, 2.000000000000830447 ) ) ;
#14222 = CARTESIAN_POINT ( 'NONE',  ( 2.071067811865476394, -24.18750000000000355, 5.000000000000000000 ) ) ;
#14223 = CARTESIAN_POINT ( 'NONE',  ( -3.033343224707664376, 3.753672977998667726, -7.999999998634409692 ) ) ;
#14224 = CARTESIAN_POINT ( 'NONE',  ( -28.86751345948129455, 1.999999999999998224, 49.99999999999999289 ) ) ;
#14225 = CARTESIAN_POINT ( 'NONE',  ( -3.535533905932738641, -25.50000000273118417, 3.535533905932737309 ) ) ;
#14226 = ORIENTED_EDGE ( 'NONE', *, *, #3559, .T. ) ;
#14227 = CARTESIAN_POINT ( 'NONE',  ( -4.458734124999999437, -26.93750000136559564, -5.460374474430324690E-16 ) ) ;
#14228 = EDGE_CURVE ( 'NONE', #13545, #3401, #5566, .T. ) ;
#14229 = DIRECTION ( 'NONE',  ( 0.000000000000000000, -1.000000000000000000, 0.000000000000000000 ) ) ;
#14230 = ORIENTED_EDGE ( 'NONE', *, *, #2350, .F. ) ;
#14231 = VERTEX_POINT ( 'NONE', #3481 ) ;
#14232 = EDGE_CURVE ( 'NONE', #6791, #6707, #7061, .T. ) ;
#14233 = CARTESIAN_POINT ( 'NONE',  ( 57.73502691896258199, -3.000000000000000000, 2.081668171172168513E-14 ) ) ;
#14234 = FACE_OUTER_BOUND ( 'NONE', #2600, .T. ) ;
#14235 = EDGE_LOOP ( 'NONE', ( #6049, #10770 ) ) ;
#14236 = DIRECTION ( 'NONE',  ( 0.000000000000000000, 0.000000000000000000, 1.000000000000000000 ) ) ;
#14237 = CARTESIAN_POINT ( 'NONE',  ( -4.211140560182196957, -2.431303136016552013, -3.745885042887436178 ) ) ;
#14238 = CARTESIAN_POINT ( 'NONE',  ( -4.458734125000001214, -27.12500000136559564, 1.846868145590734089 ) ) ;
#14239 = CARTESIAN_POINT ( 'NONE',  ( 0.5449313310647804220, 4.304185902836899835, -3.316620875263383894 ) ) ;
#14240 = APPLICATION_CONTEXT ( 'automotive_design' ) ;
#14241 = CARTESIAN_POINT ( 'NONE',  ( -91.33974596215557540, -99.99999999999995737, 17.50000000000000000 ) ) ;
#14242 = CONTEXT_DEPENDENT_SHAPE_REPRESENTATION ( #4130, #13236 ) ;
#14243 = CARTESIAN_POINT ( 'NONE',  ( -3.753672977998669946, -3.033343224707661712, -7.999999998634409692 ) ) ;
#14244 = CARTESIAN_POINT ( 'NONE',  ( 2.131511515620586383, 3.916244202832140253, -0.4374999986344086933 ) ) ;
#14245 = EDGE_CURVE ( 'NONE', #4880, #1651, #2436, .T. ) ;
#14246 = ORIENTED_EDGE ( 'NONE', *, *, #14819, .T. ) ;
#14247 = EDGE_CURVE ( 'NONE', #10561, #4719, #15887, .T. ) ;
#14248 = SURFACE_STYLE_USAGE ( .BOTH. , #15621 ) ;
#14249 = VERTEX_POINT ( 'NONE', #14484 ) ;
#14250 = CARTESIAN_POINT ( 'NONE',  ( 17.99999999999957012, -8.784126309725975241E-13, -11.50000000000000000 ) ) ;
#14251 = EDGE_LOOP ( 'NONE', ( #12675, #3751, #14837, #2665 ) ) ;
#14252 = FILL_AREA_STYLE_COLOUR ( '', #6338 ) ;
#14253 = CARTESIAN_POINT ( 'NONE',  ( 0.000000000000000000, 0.000000000000000000, -9.999999999999998224 ) ) ;
#14254 = DIRECTION ( 'NONE',  ( 0.000000000000000000, 0.000000000000000000, -1.000000000000000000 ) ) ;
#14255 = CARTESIAN_POINT ( 'NONE',  ( 3.033343224707661712, -3.753672977998669946, 1.250000001365594304 ) ) ;
#14256 =( NAMED_UNIT ( * ) PLANE_ANGLE_UNIT ( ) SI_UNIT ( $, .RADIAN. ) );
#14257 = DIRECTION ( 'NONE',  ( 0.000000000000000000, 1.000000000000000000, 0.000000000000000000 ) ) ;
#14258 = ORIENTED_EDGE ( 'NONE', *, *, #13733, .F. ) ;
#14259 = FACE_OUTER_BOUND ( 'NONE', #15583, .T. ) ;
#14260 = DIRECTION ( 'NONE',  ( -0.000000000000000000, 0.000000000000000000, 1.000000000000000000 ) ) ;
#14261 = EDGE_CURVE ( 'NONE', #9335, #10466, #7639, .T. ) ;
#14262 = DIRECTION ( 'NONE',  ( 0.000000000000000000, -1.000000000000000000, 0.000000000000000000 ) ) ;
#14263 = ORIENTED_EDGE ( 'NONE', *, *, #13414, .T. ) ;
#14264 = DIRECTION ( 'NONE',  ( 0.000000000000000000, 0.000000000000000000, -1.000000000000000000 ) ) ;
#14265 = ORIENTED_EDGE ( 'NONE', *, *, #13097, .T. ) ;
#14266 = AXIS2_PLACEMENT_3D ( 'NONE', #15537, #4452, #13166 ) ;
#14267 = EDGE_LOOP ( 'NONE', ( #11099, #8941, #1781, #3029 ) ) ;
#14268 = CARTESIAN_POINT ( 'NONE',  ( -5.000000000000000888, -30.43750000000000355, 2.071067811865474617 ) ) ;
#14269 = DIRECTION ( 'NONE',  ( 0.000000000000000000, 1.000000000000000000, 0.000000000000000000 ) ) ;
#14270 = VECTOR ( 'NONE', #11673, 1000.000000000000000 ) ;
#14271 = DIRECTION ( 'NONE',  ( -1.000000000000000000, 0.000000000000000000, 0.000000000000000000 ) ) ;
#14272 = ADVANCED_FACE ( 'NONE', ( #15787 ), #914, .F. ) ;
#14273 = DIRECTION ( 'NONE',  ( 0.000000000000000000, 0.000000000000000000, -1.000000000000000000 ) ) ;
#14274 = CARTESIAN_POINT ( 'NONE',  ( -5.725490332106779157, -5.000000000000000000, -22.00000000000000000 ) ) ;
#14275 = CARTESIAN_POINT ( 'NONE',  ( 4.000000000000000000, -1.942223658245635809, -0.3516579909967643691 ) ) ;
#14276 = DIRECTION ( 'NONE',  ( -0.000000000000000000, -0.000000000000000000, 1.000000000000000000 ) ) ;
#14277 = LINE ( 'NONE', #9280, #4739 ) ;
#14278 = VECTOR ( 'NONE', #727, 1000.000000000000000 ) ;
#14279 = DIRECTION ( 'NONE',  ( -1.000000000000000000, -0.000000000000000000, -0.000000000000000000 ) ) ;
#14280 = CARTESIAN_POINT ( 'NONE',  ( 2.730187237215162345E-16, -28.43750000136559564, -4.458734124999999437 ) ) ;
#14281 = CARTESIAN_POINT ( 'NONE',  ( 3.033343224707661712, -3.753672977998669946, -1.499999998634408138 ) ) ;
#14282 = ORIENTED_EDGE ( 'NONE', *, *, #8326, .T. ) ;
#14283 = LINE ( 'NONE', #3206, #9204 ) ;
#14284 = VERTEX_POINT ( 'NONE', #10691 ) ;
#14285 = ORIENTED_EDGE ( 'NONE', *, *, #8278, .T. ) ;
#14286 =( BOUNDED_CURVE ( )  B_SPLINE_CURVE ( 2, ( #14168, #3096, #11566, #11483, #5356, #10532, #15223, #1864, #6809, #14075, #11718 ),
 .UNSPECIFIED., .F., .F. ) 
 B_SPLINE_CURVE_WITH_KNOTS ( ( 3, 2, 2, 2, 2, 3 ),
 ( 0.8545872658012773071, 0.8625000000000000444, 0.8750000000000000000, 0.8874999999999999556, 0.9000000000000000222, 0.9045872658012773515 ),
 .UNSPECIFIED. ) 
 CURVE ( )  GEOMETRIC_REPRESENTATION_ITEM ( )  RATIONAL_B_SPLINE_CURVE ( ( 0.9646335149384808183, 0.9518143178943441196, 1.000000000000000000, 0.9238795325112867385, 1.000000000000000000, 0.9238795325112867385, 1.000000000000000000, 0.9238795325112867385, 1.000000000000000000, 0.9720652146169423968, 0.9646335149384803742 ) ) 
 REPRESENTATION_ITEM ( '' )  );
#14287 = CARTESIAN_POINT ( 'NONE',  ( -3.152801135295367096, -27.31250000136559564, -3.152801135295367541 ) ) ;
#14288 = CARTESIAN_POINT ( 'NONE',  ( -0.6920835326022555245, -4.454600218803899558, -3.597382984111586079 ) ) ;
#14289 = CARTESIAN_POINT ( 'NONE',  ( -120.0000000000000142, -106.5470053837925946, -7.500000000000000000 ) ) ;
#14290 = CARTESIAN_POINT ( 'NONE',  ( 7.499999999999654499, 3.105728215500202172, -7.659336188854535266 ) ) ;
#14291 = EDGE_CURVE ( 'NONE', #12397, #5431, #7889, .T. ) ;
#14292 = CARTESIAN_POINT ( 'NONE',  ( -3.916244202832140253, 2.131511515620587272, -5.937499998634407028 ) ) ;
#14293 = CARTESIAN_POINT ( 'NONE',  ( 2.390265326283148806, 4.391654775818395251, -5.749999997268814944 ) ) ;
#14294 = EDGE_CURVE ( 'NONE', #1787, #1633, #7635, .T. ) ;
#14295 = CARTESIAN_POINT ( 'NONE',  ( -2.071067811865478170, -26.31250000000000355, 5.000000000000000000 ) ) ;
#14296 = CARTESIAN_POINT ( 'NONE',  ( -4.391654775818395251, 2.390265326283148806, 1.374999999999997780 ) ) ;
#14297 = CARTESIAN_POINT ( 'NONE',  ( 16.49999999999956657, -8.786575603324269439E-13, 0.000000000000000000 ) ) ;
#14298 = CYLINDRICAL_SURFACE ( 'NONE', #12320, 1.999999999999998224 ) ;
#14299 = CARTESIAN_POINT ( 'NONE',  ( 4.458734124999999437, -29.50000000136559564, 1.846868145590737864 ) ) ;
#14300 = EDGE_LOOP ( 'NONE', ( #13881, #13708, #12018, #11042 ) ) ;
#14301 = DIRECTION ( 'NONE',  ( 0.000000000000000000, 0.000000000000000000, 1.000000000000000000 ) ) ;
#14302 = CARTESIAN_POINT ( 'NONE',  ( 7.779103221381269861, -4.168986698926033796, -7.929128246061908136 ) ) ;
#14303 = ORIENTED_EDGE ( 'NONE', *, *, #11046, .F. ) ;
#14304 = ORIENTED_EDGE ( 'NONE', *, *, #1060, .T. ) ;
#14305 = CARTESIAN_POINT ( 'NONE',  ( 7.500000000000000000, -3.988190556646209028, -0.8526458641284334616 ) ) ;
#14306 = STYLED_ITEM ( 'NONE', ( #14128 ), #2911 ) ;
#14307 = CARTESIAN_POINT ( 'NONE',  ( -9.184850993605147944E-16, -29.37500000273118417, 5.000000000000000000 ) ) ;
#14308 = ORIENTED_EDGE ( 'NONE', *, *, #13414, .F. ) ;
#14309 = CARTESIAN_POINT ( 'NONE',  ( -5.725490332117410652, -3.000000000000000000, 9.916840153471811803 ) ) ;
#14310 = CARTESIAN_POINT ( 'NONE',  ( -44.43375672974056556, -3.000000000000000000, 19.99999999999999645 ) ) ;
#14311 = ADVANCED_FACE ( 'NONE', ( #8520 ), #10773, .F. ) ;
#14312 = CARTESIAN_POINT ( 'NONE',  ( 1.846868145590735200, -27.50000000136559208, -4.458734125000000326 ) ) ;
#14313 = AXIS2_PLACEMENT_3D ( 'NONE', #9826, #14756, #3679 ) ;
#14314 = CARTESIAN_POINT ( 'NONE',  ( 5.200000000000002842, 0.000000000000000000, 0.000000000000000000 ) ) ;
#14315 = PLANE ( 'NONE',  #13639 ) ;
#14316 = CARTESIAN_POINT ( 'NONE',  ( 2.071067811865485275, -31.18749999999999645, 4.999999999999989342 ) ) ;
#14317 = VECTOR ( 'NONE', #12216, 1000.000000000000000 ) ;
#14318 = FACE_OUTER_BOUND ( 'NONE', #2906, .T. ) ;
#14319 = CARTESIAN_POINT ( 'NONE',  ( 6.123233995736766282E-16, -11.00000000000000178, -5.000000000000000000 ) ) ;
#14320 = ORIENTED_EDGE ( 'NONE', *, *, #15781, .T. ) ;
#14321 = ORIENTED_EDGE ( 'NONE', *, *, #7586, .F. ) ;
#14322 = CARTESIAN_POINT ( 'NONE',  ( -4.406466114817408020, 6.116179640279713503, -7.446478553995123484 ) ) ;
#14323 = STYLED_ITEM ( 'NONE', ( #13582 ), #6582 ) ;
#14324 = AXIS2_PLACEMENT_3D ( 'NONE', #12036, #2181, #4772 ) ;
#14325 = ORIENTED_EDGE ( 'NONE', *, *, #13327, .T. ) ;
#14326 = CIRCLE ( 'NONE', #5304, 7.500000000000001776 ) ;
#14327 = EDGE_CURVE ( 'NONE', #10919, #14811, #15625, .T. ) ;
#14328 = EDGE_CURVE ( 'NONE', #8368, #5406, #8625, .T. ) ;
#14329 = EDGE_CURVE ( 'NONE', #1925, #2616, #5997, .T. ) ;
#14330 = CARTESIAN_POINT ( 'NONE',  ( -2.390265326283148806, -4.391654775818394363, -3.249999997268816276 ) ) ;
#14331 = CARTESIAN_POINT ( 'NONE',  ( -3.916244202832140253, 2.131511515620587272, 0.06250000136559172303 ) ) ;
#14332 = AXIS2_PLACEMENT_3D ( 'NONE', #13077, #5810, #811 ) ;
#14333 = CARTESIAN_POINT ( 'NONE',  ( -4.795541693661363958, -1.415196051561583790, -6.374999997268815832 ) ) ;
#14334 =( LENGTH_UNIT ( ) NAMED_UNIT ( * ) SI_UNIT ( .MILLI., .METRE. ) );
#14335 = CARTESIAN_POINT ( 'NONE',  ( 5.000000000000004441, -2.247904837838113790E-16, -2.045263047592944528 ) ) ;
#14336 = CARTESIAN_POINT ( 'NONE',  ( -36.99999999999999289, -13.00000000000000178, 2.000000000000830891 ) ) ;
#14337 = ORIENTED_EDGE ( 'NONE', *, *, #8793, .F. ) ;
#14338 = CIRCLE ( 'NONE', #7373, 5.000000000000000000 ) ;
#14339 = DIRECTION ( 'NONE',  ( 0.000000000000000000, 0.000000000000000000, -1.000000000000000000 ) ) ;
#14340 = CARTESIAN_POINT ( 'NONE',  ( 4.795541693661363958, 1.415196051561583790, -2.874999997268815832 ) ) ;
#14341 = CARTESIAN_POINT ( 'NONE',  ( -43.99999999999978684, -9.000000000000001776, -1.500000000000000666 ) ) ;
#14342 = ORIENTED_EDGE ( 'NONE', *, *, #2127, .F. ) ;
#14343 = CARTESIAN_POINT ( 'NONE',  ( 9.184850993605150311E-15, 40.00000000000000000, -75.00000000000001421 ) ) ;
#14344 = ORIENTED_EDGE ( 'NONE', *, *, #11089, .T. ) ;
#14345 = VERTEX_POINT ( 'NONE', #13411 ) ;
#14346 = CARTESIAN_POINT ( 'NONE',  ( -21.01110699893041556, -1.230770033143087371E-15, -39.04230484541333368 ) ) ;
#14347 = CYLINDRICAL_SURFACE ( 'NONE', #5843, 2.500000000000909495 ) ;
#14348 = AXIS2_PLACEMENT_3D ( 'NONE', #2453, #4816, #8549 ) ;
#14349 = CARTESIAN_POINT ( 'NONE',  ( -4.000000000000000000, 2.309401076758498483, -5.000000000000000000 ) ) ;
#14350 = CIRCLE ( 'NONE', #8669, 25.00000000000000000 ) ;
#14351 = EDGE_CURVE ( 'NONE', #7200, #15077, #3731, .T. ) ;
#14352 = APPLICATION_CONTEXT ( 'automotive_design' ) ;
#14353 = CYLINDRICAL_SURFACE ( 'NONE', #12802, 5.000000000000000000 ) ;
#14354 = FACE_BOUND ( 'NONE', #3333, .T. ) ;
#14355 = CARTESIAN_POINT ( 'NONE',  ( 25.00000000000000000, 0.000000000000000000, 2.055000000000000160 ) ) ;
#14356 = CARTESIAN_POINT ( 'NONE',  ( 35.00000000000000000, 40.00000000000000000, -8.572527594031472993E-15 ) ) ;
#14357 = LINE ( 'NONE', #14439, #9631 ) ;
#14358 = CARTESIAN_POINT ( 'NONE',  ( 2.071067811865505259, -25.31250000273118062, 4.999999999999970690 ) ) ;
#14359 = CARTESIAN_POINT ( 'NONE',  ( -4.458734124999999437, -30.18750000136559564, -5.460374474430324690E-16 ) ) ;
#14360 = CARTESIAN_POINT ( 'NONE',  ( -4.276409079477644148, -1.261996585732578335, 1.187500001365592750 ) ) ;
#14361 = EDGE_LOOP ( 'NONE', ( #9794, #12439, #6732, #14461 ) ) ;
#14362 = CARTESIAN_POINT ( 'NONE',  ( 5.147825380264579920, 5.688155668807426402, -7.450218641349906079 ) ) ;
#14363 = ORIENTED_EDGE ( 'NONE', *, *, #9169, .F. ) ;
#14364 = ORIENTED_EDGE ( 'NONE', *, *, #819, .F. ) ;
#14365 = CIRCLE ( 'NONE', #9464, 25.00000000000000000 ) ;
#14366 = CARTESIAN_POINT ( 'NONE',  ( 2.730187237215162345E-16, -26.43750000136559564, -4.458734124999999437 ) ) ;
#14367 = CARTESIAN_POINT ( 'NONE',  ( 2.390265326283148806, 4.391654775818395251, -7.875000000000003553 ) ) ;
#14368 = MANIFOLD_SOLID_BREP ( 'Boss-Extrude3', #8186 ) ;
#14369 = LINE ( 'NONE', #15669, #4284 ) ;
#14370 = AXIS2_PLACEMENT_3D ( 'NONE', #10963, #15906, #8557 ) ;
#14371 = CARTESIAN_POINT ( 'NONE',  ( -4.799145180956616130, 0.5093500532425063732, -7.874999998634408804 ) ) ;
#14372 = CARTESIAN_POINT ( 'NONE',  ( -4.799145180956616130, 0.5093500532425063732, -5.874999998634406140 ) ) ;
#14373 = CARTESIAN_POINT ( 'NONE',  ( 4.199643060765958502, -3.477892933143082121, 48.66604890908090653 ) ) ;
#14374 = PRODUCT_DEFINITION_FORMATION_WITH_SPECIFIED_SOURCE ( 'ANY', '', #13106, .NOT_KNOWN. ) ;
#14375 = AXIS2_PLACEMENT_3D ( 'NONE', #7579, #14931, #3850 ) ;
#14376 = CARTESIAN_POINT ( 'NONE',  ( -5.000000000000000000, -26.50000000000000355, -6.123233995736766282E-16 ) ) ;
#14377 = AXIS2_PLACEMENT_3D ( 'NONE', #13919, #11340, #11256 ) ;
#14378 = CARTESIAN_POINT ( 'NONE',  ( 5.381735091635035495, -0.5711823568785978633, 1.937499999999998890 ) ) ;
#14379 = FACE_BOUND ( 'NONE', #15102, .T. ) ;
#14380 = DIRECTION ( 'NONE',  ( 0.000000000000000000, 0.000000000000000000, 1.000000000000000000 ) ) ;
#14381 = CARTESIAN_POINT ( 'NONE',  ( -4.458734125000000326, -29.00000000136559564, -1.846868145590735644 ) ) ;
#14382 = B_SPLINE_CURVE_WITH_KNOTS ( 'NONE', 3,
 ( #5571, #8010, #5798, #3376, #3302, #2004 ),
 .UNSPECIFIED., .F., .F.,
 ( 4, 2, 4 ),
 ( 2.475503369269340592E-07, 0.002222330217055639313, 0.004444412883774352327 ),
 .UNSPECIFIED. ) ;
#14383 = ORIENTED_EDGE ( 'NONE', *, *, #13542, .F. ) ;
#14384 = CARTESIAN_POINT ( 'NONE',  ( 9.184850993605153466E-15, 50.00000000000000000, 75.00000000000004263 ) ) ;
#14385 = DIRECTION ( 'NONE',  ( 1.000000000000000000, 0.000000000000000000, 0.000000000000000000 ) ) ;
#14386 = ORIENTED_EDGE ( 'NONE', *, *, #7006, .T. ) ;
#14387 = AXIS2_PLACEMENT_3D ( 'NONE', #368, #5283, #10223 ) ;
#14388 = EDGE_LOOP ( 'NONE', ( #5874, #4605, #5184 ) ) ;
#14389 = CARTESIAN_POINT ( 'NONE',  ( 1.393927851585479161, -4.043713361053543842, -3.526374918436840922 ) ) ;
#14390 = CARTESIAN_POINT ( 'NONE',  ( -3.152801135295367985, -26.81250000136559564, 3.152801135295367096 ) ) ;
#14391 = EDGE_CURVE ( 'NONE', #4663, #12836, #11907, .T. ) ;
#14392 = FACE_OUTER_BOUND ( 'NONE', #1951, .T. ) ;
#14393 = EDGE_CURVE ( 'NONE', #3118, #15938, #8924, .T. ) ;
#14394 = VERTEX_POINT ( 'NONE', #14551 ) ;
#14395 = DIRECTION ( 'NONE',  ( 1.000000000000000000, 0.000000000000000000, 0.000000000000000000 ) ) ;
#14396 = CIRCLE ( 'NONE', #6651, 3.499999999999999556 ) ;
#14397 = CARTESIAN_POINT ( 'NONE',  ( 39.84845309559526072, -3.761076017575720964, -28.17072103117275716 ) ) ;
#14398 = CARTESIAN_POINT ( 'NONE',  ( 1.846868145590735200, -28.50000000136559564, -4.458734125000000326 ) ) ;
#14399 = CARTESIAN_POINT ( 'NONE',  ( 4.140404888673277384, 2.228338276487440428, -3.686887068327033390 ) ) ;
#14400 = CARTESIAN_POINT ( 'NONE',  ( 5.000000000000002665, 1.275685995473128912E-14, -4.045263047592942307 ) ) ;
#14401 = FACE_OUTER_BOUND ( 'NONE', #8295, .T. ) ;
#14402 = VECTOR ( 'NONE', #14301, 1000.000000000000000 ) ;
#14403 = DIRECTION ( 'NONE',  ( 0.000000000000000000, 1.000000000000000000, 0.000000000000000000 ) ) ;
#14404 = CIRCLE ( 'NONE', #15175, 1.999999999999998224 ) ;
#14405 = EDGE_LOOP ( 'NONE', ( #12617, #6142, #12154, #4288, #2310, #3462 ) ) ;
#14406 =( LENGTH_UNIT ( ) NAMED_UNIT ( * ) SI_UNIT ( .MILLI., .METRE. ) );
#14407 = AXIS2_PLACEMENT_3D ( 'NONE', #9200, #14204, #3127 ) ;
#14409 = ORIENTED_EDGE ( 'NONE', *, *, #183, .T. ) ;
#14408 = ADVANCED_FACE ( 'NONE', ( #4691 ), #11878, .T. ) ;
#14410 = CARTESIAN_POINT ( 'NONE',  ( 0.3470952277635127037, 8.860649561028118626, -7.493596212620251329 ) ) ;
#14411 = EDGE_CURVE ( 'NONE', #11470, #7943, #14845, .T. ) ;
#14412 = VERTEX_POINT ( 'NONE', #13243 ) ;
#14413 = CARTESIAN_POINT ( 'NONE',  ( -5.000000000000000888, -26.43750000000000711, 2.071067811865474617 ) ) ;
#14414 = DIRECTION ( 'NONE',  ( 0.000000000000000000, 0.000000000000000000, -1.000000000000000000 ) ) ;
#14415 = CARTESIAN_POINT ( 'NONE',  ( 4.799145180956616130, -0.5093500532425063732, 1.625000001365592528 ) ) ;
#14416 = CARTESIAN_POINT ( 'NONE',  ( 10.00000000000033751, -13.50000000000000178, -17.32050807568907658 ) ) ;
#14417 = CARTESIAN_POINT ( 'NONE',  ( 2.131511515620586383, 3.916244202832140253, -3.437499998634407916 ) ) ;
#14418 = CARTESIAN_POINT ( 'NONE',  ( 5.000000000000004441, 6.350331166892669572E-15, -1.045263047592943417 ) ) ;
#14419 = CARTESIAN_POINT ( 'NONE',  ( -9.184850993605147944E-16, -22.37500000273118417, 5.000000000000000000 ) ) ;
#14420 = VERTEX_POINT ( 'NONE', #4535 ) ;
#14421 = DIRECTION ( 'NONE',  ( 0.000000000000000000, 0.000000000000000000, 1.000000000000000000 ) ) ;
#14422 = CARTESIAN_POINT ( 'NONE',  ( 24.26932219902320043, 40.00000000000000000, -5.999999999999989342 ) ) ;
#14423 = AXIS2_PLACEMENT_3D ( 'NONE', #15311, #12778, #4146 ) ;
#14424 = ADVANCED_FACE ( 'NONE', ( #9549 ), #14477, .F. ) ;
#14425 = VERTEX_POINT ( 'NONE', #10839 ) ;
#14426 = CARTESIAN_POINT ( 'NONE',  ( 35.00000000000000000, 40.00000000000000000, 5.999999999999991118 ) ) ;
#14427 = ORIENTED_EDGE ( 'NONE', *, *, #8832, .F. ) ;
#14428 = ADVANCED_FACE ( 'NONE', ( #14401 ), #13547, .T. ) ;
#14429 = VERTEX_POINT ( 'NONE', #4096 ) ;
#14430 = CARTESIAN_POINT ( 'NONE',  ( -2.131511515620587272, -3.916244202832140253, -0.9374999986344056957 ) ) ;
#14431 = DIRECTION ( 'NONE',  ( 0.000000000000000000, 0.000000000000000000, -1.000000000000000000 ) ) ;
#14432 = AXIS2_PLACEMENT_3D ( 'NONE', #784, #11837, #11520 ) ;
#14433 = VECTOR ( 'NONE', #12995, 1000.000000000000114 ) ;
#14434 = DIRECTION ( 'NONE',  ( 0.000000000000000000, 0.000000000000000000, -1.000000000000000000 ) ) ;
#14435 = CARTESIAN_POINT ( 'NONE',  ( 35.00000000000000000, 37.00000000000000000, -5.999999999999991118 ) ) ;
#14436 = DIRECTION ( 'NONE',  ( 0.000000000000000000, 0.000000000000000000, 1.000000000000000000 ) ) ;
#14437 = CARTESIAN_POINT ( 'NONE',  ( 3.999999999999999112, -0.3979232138631231819, -5.929230630780099908E-17 ) ) ;
#14438 = CARTESIAN_POINT ( 'NONE',  ( 0.2500000000000002220, 0.000000000000000000, 0.000000000000000000 ) ) ;
#14439 = CARTESIAN_POINT ( 'NONE',  ( 0.000000000000000000, -13.00000000000000178, -5.000000000000000000 ) ) ;
#14440 = DIRECTION ( 'NONE',  ( -0.005931855436079011210, 0.9999824063907751803, 0.000000000000000000 ) ) ;
#14441 = CARTESIAN_POINT ( 'NONE',  ( 1.846868145590735200, -28.50000000136559564, -4.458734124999999437 ) ) ;
#14442 = CARTESIAN_POINT ( 'NONE',  ( 4.799145180956616130, -0.5093500532425063732, -1.374999998634406140 ) ) ;
#14443 = ORIENTED_EDGE ( 'NONE', *, *, #6203, .F. ) ;
#14444 = AXIS2_PLACEMENT_3D ( 'NONE', #6999, #4408, #5620 ) ;
#14445 = ADVANCED_FACE ( 'NONE', ( #556 ), #7832, .T. ) ;
#14446 = EDGE_LOOP ( 'NONE', ( #2969, #6183, #11392, #10040 ) ) ;
#14447 = ORIENTED_EDGE ( 'NONE', *, *, #83, .F. ) ;
#14448 = EDGE_CURVE ( 'NONE', #13155, #9599, #15341, .T. ) ;
#14449 = PRODUCT_CONTEXT ( 'NONE', #8986, 'mechanical' ) ;
#14450 = ORIENTED_EDGE ( 'NONE', *, *, #8123, .F. ) ;
#14451 = CARTESIAN_POINT ( 'NONE',  ( -1.846868145590734756, -26.37500000136559564, -4.458734125000000326 ) ) ;
#14452 = CARTESIAN_POINT ( 'NONE',  ( -2.071067811865475061, -23.81250000273118772, -5.000000000000000888 ) ) ;
#14453 = DIRECTION ( 'NONE',  ( 0.000000000000000000, 0.000000000000000000, 1.000000000000000000 ) ) ;
#14454 = DIRECTION ( 'NONE',  ( 0.000000000000000000, 0.000000000000000000, 1.000000000000000000 ) ) ;
#14455 = LINE ( 'NONE', #10420, #14278 ) ;
#14456 = CARTESIAN_POINT ( 'NONE',  ( 5.000000000000000000, -22.00000000000000000, 0.000000000000000000 ) ) ;
#14457 = CARTESIAN_POINT ( 'NONE',  ( 1.261996585732578113, -4.276409079477644148, -6.562499998634407028 ) ) ;
#14458 = CARTESIAN_POINT ( 'NONE',  ( -3.535533905932737309, -21.75000000273118772, -3.535533905932738197 ) ) ;
#14459 = CARTESIAN_POINT ( 'NONE',  ( 0.2323655586075058233, -4.874496464951329600, -0.08906361846652831316 ) ) ;
#14460 = CARTESIAN_POINT ( 'NONE',  ( -2.071067811865478170, -21.43750000273119127, 5.000000000000000000 ) ) ;
#14461 = ORIENTED_EDGE ( 'NONE', *, *, #7006, .F. ) ;
#14462 = LINE ( 'NONE', #8334, #7370 ) ;
#14463 = ORIENTED_EDGE ( 'NONE', *, *, #8743, .F. ) ;
#14464 = VERTEX_POINT ( 'NONE', #15262 ) ;
#14465 = CARTESIAN_POINT ( 'NONE',  ( 0.000000000000000000, 20.00000000000000000, 25.00000000000000000 ) ) ;
#14466 = EDGE_CURVE ( 'NONE', #9203, #6666, #3048, .T. ) ;
#14467 = CARTESIAN_POINT ( 'NONE',  ( 3.152801135295367541, -27.31250000136559564, -3.152801135295367541 ) ) ;
#14468 = CARTESIAN_POINT ( 'NONE',  ( 42.02221399786069611, -1.230770033143087371E-15, 2.650000000000093170 ) ) ;
#14469 = ORIENTED_EDGE ( 'NONE', *, *, #3722, .F. ) ;
#14470 = CARTESIAN_POINT ( 'NONE',  ( 19.99999999999956657, -8.786575603324269439E-13, 0.000000000000000000 ) ) ;
#14471 = FACE_BOUND ( 'NONE', #10823, .T. ) ;
#14472 = DIRECTION ( 'NONE',  ( 0.000000000000000000, 0.000000000000000000, 1.000000000000000000 ) ) ;
#14473 = CARTESIAN_POINT ( 'NONE',  ( 4.458734124999999437, -23.75000000136559208, 1.846868145590737864 ) ) ;
#14474 = CYLINDRICAL_SURFACE ( 'NONE', #15292, 2.500000000000000444 ) ;
#14475 = EDGE_CURVE ( 'NONE', #12864, #12101, #5140, .T. ) ;
#14476 = CARTESIAN_POINT ( 'NONE',  ( 5.000000000000004441, 0.000000000000000000, 0.000000000000000000 ) ) ;
#14477 = PLANE ( 'NONE',  #5808 ) ;
#14478 = CARTESIAN_POINT ( 'NONE',  ( 4.197393957002303999, 7.772902908466098641E-14, -3.503767560748929810 ) ) ;
#14479 = ORIENTED_EDGE ( 'NONE', *, *, #8065, .F. ) ;
#14480 = SHAPE_REPRESENTATION_RELATIONSHIP ( 'NONE' , 'NONE' ,  #396, #6973 ) ;
#14481 = ORIENTED_EDGE ( 'NONE', *, *, #13427, .F. ) ;
#14482 = CARTESIAN_POINT ( 'NONE',  ( 11.91154273188008084, 0.000000000000000000, 56.63139720814412925 ) ) ;
#14483 = EDGE_LOOP ( 'NONE', ( #9675, #1193, #1974, #4410 ) ) ;
#14484 = CARTESIAN_POINT ( 'NONE',  ( 16.49999999999956657, -8.786575603324269439E-13, 1.500000000000000000 ) ) ;
#14485 = CARTESIAN_POINT ( 'NONE',  ( 0.000000000000000000, -13.00000000000000178, 0.000000000000000000 ) ) ;
#14486 = ADVANCED_FACE ( 'NONE', ( #7887 ), #5289, .F. ) ;
#14487 = CARTESIAN_POINT ( 'NONE',  ( -4.799145180956616130, 0.5093500532425063732, -0.8749999986344056957 ) ) ;
#14488 = EDGE_CURVE ( 'NONE', #12412, #8728, #8857, .T. ) ;
#14489 = CARTESIAN_POINT ( 'NONE',  ( 0.000000000000000000, 0.000000000000000000, 0.000000000000000000 ) ) ;
#14490 = CARTESIAN_POINT ( 'NONE',  ( 3.753672977998667726, 3.033343224707664376, -0.4999999986344072500 ) ) ;
#14491 = CARTESIAN_POINT ( 'NONE',  ( 0.000000000000000000, 0.000000000000000000, -25.03750572909317285 ) ) ;
#14492 = PRESENTATION_STYLE_ASSIGNMENT (( #7233 ) ) ;
#14493 = ORIENTED_EDGE ( 'NONE', *, *, #5242, .T. ) ;
#14494 = CARTESIAN_POINT ( 'NONE',  ( -2.071067811865450192, -22.31250000000000000, 5.000000000000028422 ) ) ;
#14495 = DIRECTION ( 'NONE',  ( 0.000000000000000000, 0.4999999999999993339, -0.8660254037844390407 ) ) ;
#14496 = VERTEX_POINT ( 'NONE', #7969 ) ;
#14497 = CARTESIAN_POINT ( 'NONE',  ( 5.000000000000000888, 0.000000000000000000, -25.03750572909317285 ) ) ;
#14498 = ORIENTED_EDGE ( 'NONE', *, *, #8511, .T. ) ;
#14499 = ORIENTED_EDGE ( 'NONE', *, *, #7024, .F. ) ;
#14500 = CARTESIAN_POINT ( 'NONE',  ( -5.000000000000004441, -7.530481206757679743E-15, -2.420263044861759472 ) ) ;
#14501 = VECTOR ( 'NONE', #10909, 1000.000000000000114 ) ;
#14502 = DIRECTION ( 'NONE',  ( 0.000000000000000000, 0.000000000000000000, 1.000000000000000000 ) ) ;
#14503 = EDGE_CURVE ( 'NONE', #349, #9262, #3988, .T. ) ;
#14504 = CARTESIAN_POINT ( 'NONE',  ( 2.500000000000000000, 2.357898499370433054, -1.951563910473907981E-15 ) ) ;
#14505 = DIRECTION ( 'NONE',  ( 0.8660254037844401509, -0.4999999999999973355, 0.000000000000000000 ) ) ;
#14506 = EDGE_CURVE ( 'NONE', #2790, #10935, #4073, .T. ) ;
#14507 = LINE ( 'NONE', #7009, #1518 ) ;
#14508 = CARTESIAN_POINT ( 'NONE',  ( -4.336808689942016257E-16, -8.660254037844397956, -7.564338275809346257 ) ) ;
#14509 = LINE ( 'NONE', #5949, #12339 ) ;
#14510 = DIRECTION ( 'NONE',  ( 0.000000000000000000, 0.000000000000000000, 1.000000000000000000 ) ) ;
#14511 = CARTESIAN_POINT ( 'NONE',  ( 2.730187237215162345E-16, -29.43750000136559208, -4.458734124999999437 ) ) ;
#14512 = CARTESIAN_POINT ( 'NONE',  ( 3.033343224707661712, -3.753672977998669946, 0.5000000013655936382 ) ) ;
#14513 = ORIENTED_EDGE ( 'NONE', *, *, #1683, .F. ) ;
#14514 = DIRECTION ( 'NONE',  ( -0.000000000000000000, -1.000000000000000000, -0.000000000000000000 ) ) ;
#14515 = ORIENTED_EDGE ( 'NONE', *, *, #8862, .T. ) ;
#14516 = VECTOR ( 'NONE', #4314, 1000.000000000000000 ) ;
#14517 = ORIENTED_EDGE ( 'NONE', *, *, #7117, .T. ) ;
#14518 = SHAPE_REPRESENTATION_RELATIONSHIP ( 'NONE' , 'NONE' ,  #790, #7752 ) ;
#14519 = ORIENTED_EDGE ( 'NONE', *, *, #4767, .F. ) ;
#14520 = CARTESIAN_POINT ( 'NONE',  ( 4.458734125000000326, -28.62500000136559919, -1.846868145590734978 ) ) ;
#14521 = CARTESIAN_POINT ( 'NONE',  ( -2.071067811865478170, -23.43750000273119127, 5.000000000000000000 ) ) ;
#14522 = FACE_BOUND ( 'NONE', #3894, .T. ) ;
#14523 = AXIS2_PLACEMENT_3D ( 'NONE', #12594, #2901, #7852 ) ;
#14524 = EDGE_CURVE ( 'NONE', #7180, #8026, #11729, .T. ) ;
#14525 = AXIS2_PLACEMENT_3D ( 'NONE', #13617, #9592, #14690 ) ;
#14526 = DIRECTION ( 'NONE',  ( 0.8660254037844401509, -0.4999999999999973355, 0.000000000000000000 ) ) ;
#14527 = DIRECTION ( 'NONE',  ( 1.000000000000000000, 0.000000000000000000, 0.000000000000000000 ) ) ;
#14528 = EDGE_CURVE ( 'NONE', #9656, #6965, #9933, .T. ) ;
#14529 = ADVANCED_FACE ( 'NONE', ( #11351 ), #301, .F. ) ;
#14530 = CARTESIAN_POINT ( 'NONE',  ( 4.458734124999999437, -31.43750000136559564, 0.000000000000000000 ) ) ;
#14531 = CARTESIAN_POINT ( 'NONE',  ( 2.390265326283148806, 4.391654775818395251, 0.1249999999999966416 ) ) ;
#14532 = DIRECTION ( 'NONE',  ( 0.000000000000000000, 0.000000000000000000, -1.000000000000000000 ) ) ;
#14533 = CARTESIAN_POINT ( 'NONE',  ( -0.5688975254463102260, -4.825649467606618614, -0.1037993411750909034 ) ) ;
#14534 = CARTESIAN_POINT ( 'NONE',  ( 1.846868145590735200, -30.25000000136559564, -4.458734125000000326 ) ) ;
#14535 = VERTEX_POINT ( 'NONE', #1573 ) ;
#14536 = CARTESIAN_POINT ( 'NONE',  ( -5.000000000000000888, 6.123233995736767268E-16, 0.000000000000000000 ) ) ;
#14537 = EDGE_LOOP ( 'NONE', ( #9844, #4099, #12638, #4311, #15471 ) ) ;
#14538 = EDGE_LOOP ( 'NONE', ( #11917, #14059, #15005 ) ) ;
#14539 = CARTESIAN_POINT ( 'NONE',  ( -7.500000000000003553, -3.105855721450407447, -7.659356991635974943 ) ) ;
#14540 = CARTESIAN_POINT ( 'NONE',  ( -4.458734125000000326, -30.00000000136559564, -1.846868145590735644 ) ) ;
#14541 = DIRECTION ( 'NONE',  ( 0.000000000000000000, -0.5000000000000012212, -0.8660254037844380415 ) ) ;
#14542 = ORIENTED_EDGE ( 'NONE', *, *, #14213, .F. ) ;
#14543 = CARTESIAN_POINT ( 'NONE',  ( 67.49999999999931788, 50.00000000000000000, 2.081668171172168513E-14 ) ) ;
#14544 = CARTESIAN_POINT ( 'NONE',  ( -2.459698528280934049, 7.240146430416067425, -0.09933465333851286549 ) ) ;
#14545 = DIRECTION ( 'NONE',  ( 0.000000000000000000, 0.000000000000000000, 1.000000000000000000 ) ) ;
#14546 = CARTESIAN_POINT ( 'NONE',  ( -19.99999999999956657, -9.000000000000001776, 8.786575603324269439E-13 ) ) ;
#14547 = EDGE_CURVE ( 'NONE', #2497, #15821, #3478, .T. ) ;
#14548 = CARTESIAN_POINT ( 'NONE',  ( -4.458734125000000326, -24.25000000136559564, -1.846868145590735644 ) ) ;
#14549 = CARTESIAN_POINT ( 'NONE',  ( 4.235886605889389145, 2.417314728048528760, -3.751161874094018245 ) ) ;
#14550 = DIRECTION ( 'NONE',  ( 0.000000000000000000, 0.000000000000000000, -1.000000000000000000 ) ) ;
#14551 = CARTESIAN_POINT ( 'NONE',  ( -4.336808689942017736E-16, -8.660254037844399733, -7.422398894150038728 ) ) ;
#14552 = CARTESIAN_POINT ( 'NONE',  ( -90.00000000000000000, -95.00000000000000000, 17.50000000000000000 ) ) ;
#14553 = ORIENTED_EDGE ( 'NONE', *, *, #13397, .T. ) ;
#14554 =( NAMED_UNIT ( * ) PLANE_ANGLE_UNIT ( ) SI_UNIT ( $, .RADIAN. ) );
#14555 = ORIENTED_EDGE ( 'NONE', *, *, #11906, .T. ) ;
#14556 = DIRECTION ( 'NONE',  ( 0.000000000000000000, 0.000000000000000000, 1.000000000000000000 ) ) ;
#14557 = EDGE_LOOP ( 'NONE', ( #11319, #9809, #10232, #13248, #11922, #10830, #3863, #3354, #15510, #4157, #8767, #9323, #14212, #15491, #9882, #7121, #1728, #1355, #11071, #12078, #795 ) ) ;
#14558 = EDGE_CURVE ( 'NONE', #12414, #379, #15236, .T. ) ;
#14559 = CARTESIAN_POINT ( 'NONE',  ( 2.500000000000000000, 1.178949249685213863, -2.042000000000001148 ) ) ;
#14560 = AXIS2_PLACEMENT_3D ( 'NONE', #11859, #6958, #14532 ) ;
#14561 = CARTESIAN_POINT ( 'NONE',  ( -21.01110699893041556, 2.000000000000000000, -39.04230484541333368 ) ) ;
#14562 = CARTESIAN_POINT ( 'NONE',  ( 3.033343224707661712, -3.753672977998669946, 0.5000000013655936382 ) ) ;
#14563 = DIRECTION ( 'NONE',  ( 0.000000000000000000, 0.000000000000000000, 1.000000000000000000 ) ) ;
#14564 = CARTESIAN_POINT ( 'NONE',  ( -3.033343224707664376, 3.753672977998667726, -1.249999998634407916 ) ) ;
#14565 = FILL_AREA_STYLE ('',( #14731 ) ) ;
#14566 = ORIENTED_EDGE ( 'NONE', *, *, #11025, .T. ) ;
#14567 = DIRECTION ( 'NONE',  ( 0.000000000000000000, 1.000000000000000000, 0.000000000000000000 ) ) ;
#14568 = AXIS2_PLACEMENT_3D ( 'NONE', #13417, #8444, #12202 ) ;
#14569 = SURFACE_STYLE_USAGE ( .BOTH. , #3732 ) ;
#14570 = EDGE_LOOP ( 'NONE', ( #11412, #987, #3883, #12656 ) ) ;
#14571 = ORIENTED_EDGE ( 'NONE', *, *, #1483, .F. ) ;
#14572 = AXIS2_PLACEMENT_3D ( 'NONE', #1010, #15806, #6186 ) ;
#14573 = ORIENTED_EDGE ( 'NONE', *, *, #3975, .T. ) ;
#14574 = CARTESIAN_POINT ( 'NONE',  ( 4.799145180956616130, -0.5093500532425063732, -2.624999998634407028 ) ) ;
#14575 = EDGE_CURVE ( 'NONE', #12489, #9186, #14185, .T. ) ;
#14576 = EDGE_CURVE ( 'NONE', #5972, #11644, #10464, .T. ) ;
#14577 = DIRECTION ( 'NONE',  ( 0.000000000000000000, 1.000000000000000000, 0.000000000000000000 ) ) ;
#14578 = MECHANICAL_DESIGN_GEOMETRIC_PRESENTATION_REPRESENTATION (  '', ( #3998 ), #9673 ) ;
#14579 = CIRCLE ( 'NONE', #8143, 2.649999999999985700 ) ;
#14580 = CARTESIAN_POINT ( 'NONE',  ( 4.896370289192182312, -3.000000000000000000, -48.48076211352908871 ) ) ;
#14581 = LINE ( 'NONE', #10797, #13978 ) ;
#14582 = AXIS2_PLACEMENT_3D ( 'NONE', #3406, #13176, #11886 ) ;
#14583 = CARTESIAN_POINT ( 'NONE',  ( 4.000000000000000000, 0.000000000000000000, 0.000000000000000000 ) ) ;
#14584 = CARTESIAN_POINT ( 'NONE',  ( -0.5711823568785978633, -5.381735091635035495, -1.187499997268816054 ) ) ;
#14585 = FILL_AREA_STYLE ('',( #6106 ) ) ;
#14586 =( LENGTH_UNIT ( ) NAMED_UNIT ( * ) SI_UNIT ( .MILLI., .METRE. ) );
#14587 = CARTESIAN_POINT ( 'NONE',  ( 1.846868145590736310, -24.87500000136559564, 4.458734124999997661 ) ) ;
#14588 = CARTESIAN_POINT ( 'NONE',  ( -4.276409079477644148, -1.261996585732578335, -5.812499998634406140 ) ) ;
#14589 = VERTEX_POINT ( 'NONE', #15558 ) ;
#14590 = DIRECTION ( 'NONE',  ( 0.000000000000000000, 0.000000000000000000, 1.000000000000000000 ) ) ;
#14591 = ORIENTED_EDGE ( 'NONE', *, *, #12282, .F. ) ;
#14592 = VERTEX_POINT ( 'NONE', #3641 ) ;
#14594 = AXIS2_PLACEMENT_3D ( 'NONE', #4596, #4755, #13226 ) ;
#14593 =( NAMED_UNIT ( * ) PLANE_ANGLE_UNIT ( ) SI_UNIT ( $, .RADIAN. ) );
#14595 = ORIENTED_EDGE ( 'NONE', *, *, #11128, .T. ) ;
#14596 = CARTESIAN_POINT ( 'NONE',  ( 1.846868145590736310, -21.87500000136559208, 4.458734124999999437 ) ) ;
#14597 = DIRECTION ( 'NONE',  ( 1.000000000000000000, 0.000000000000000000, 0.000000000000000000 ) ) ;
#14598 = EDGE_CURVE ( 'NONE', #10519, #5083, #12504, .T. ) ;
#14599 = CIRCLE ( 'NONE', #6086, 7.500000000000001776 ) ;
#14600 = AXIS2_PLACEMENT_3D ( 'NONE', #2728, #6624, #8810 ) ;
#14601 = FACE_BOUND ( 'NONE', #8788, .T. ) ;
#14602 = CARTESIAN_POINT ( 'NONE',  ( -4.618802153517017395, -5.000000000000000000, 36.00000000000000711 ) ) ;
#14603 = CARTESIAN_POINT ( 'NONE',  ( 0.000000000000000000, 50.00000000000000000, 0.000000000000000000 ) ) ;
#14604 =( BOUNDED_CURVE ( )  B_SPLINE_CURVE ( 3, ( #6139, #14703, #12256, #4599 ),
 .UNSPECIFIED., .F., .F. ) 
 B_SPLINE_CURVE_WITH_KNOTS ( ( 4, 4 ),
 ( 1.570796326794896558, 3.141592653589793116 ),
 .UNSPECIFIED. ) 
 CURVE ( )  GEOMETRIC_REPRESENTATION_ITEM ( )  RATIONAL_B_SPLINE_CURVE ( ( 1.000000000000000000, 0.8047378541243649375, 0.8047378541243649375, 1.000000000000000000 ) ) 
 REPRESENTATION_ITEM ( '' )  );
#14605 = CARTESIAN_POINT ( 'NONE',  ( -9.184850993605147944E-16, -23.25000000000000000, 5.000000000000000000 ) ) ;
#14606 = VECTOR ( 'NONE', #394, 1000.000000000000000 ) ;
#14607 = CARTESIAN_POINT ( 'NONE',  ( 4.795541693661363958, 1.415196051561583790, -2.000000000000001776 ) ) ;
#14608 = CARTESIAN_POINT ( 'NONE',  ( -2.390265326283148806, -4.391654775818394363, -2.249999997268815388 ) ) ;
#14609 = CARTESIAN_POINT ( 'NONE',  ( -4.586482550153569981, -1.057820282786336108, -0.2105217688629980877 ) ) ;
#14610 = CARTESIAN_POINT ( 'NONE',  ( -4.458734124999999437, -29.93750000136559564, -5.460374474430324690E-16 ) ) ;
#14611 = CIRCLE ( 'NONE', #8437, 2.055000000000000160 ) ;
#14612 = B_SPLINE_CURVE_WITH_KNOTS ( 'NONE', 3,
 ( #10588, #14288, #5565, #3059, #4184, #8159, #876, #3210 ),
 .UNSPECIFIED., .F., .F.,
 ( 4, 2, 2, 4 ),
 ( 0.000000000000000000, 0.002450665683189818828, 0.003675998524784728459, 0.004901331366379638524 ),
 .UNSPECIFIED. ) ;
#14613 = CARTESIAN_POINT ( 'NONE',  ( 3.916244202832140253, -2.131511515620588160, -2.687499998634407028 ) ) ;
#14614 = ORIENTED_EDGE ( 'NONE', *, *, #2414, .T. ) ;
#14615 = LINE ( 'NONE', #4675, #10213 ) ;
#14616 = ORIENTED_EDGE ( 'NONE', *, *, #14817, .F. ) ;
#14617 = ORIENTED_EDGE ( 'NONE', *, *, #1683, .T. ) ;
#14618 = PLANE ( 'NONE',  #4378 ) ;
#14619 = CARTESIAN_POINT ( 'NONE',  ( -8.190561711645485556E-16, -23.68750000136559564, 4.458734124999999437 ) ) ;
#14620 = EDGE_CURVE ( 'NONE', #13915, #4440, #14579, .T. ) ;
#14621 = CARTESIAN_POINT ( 'NONE',  ( -91.28042740779480368, -120.0589677227266918, 7.500000000000001776 ) ) ;
#14622 = EDGE_CURVE ( 'NONE', #13190, #14775, #1807, .T. ) ;
#14623 = ADVANCED_FACE ( 'NONE', ( #4475 ), #11658, .T. ) ;
#14624 = ORIENTED_EDGE ( 'NONE', *, *, #5507, .F. ) ;
#14625 = FACE_OUTER_BOUND ( 'NONE', #15142, .T. ) ;
#14626 = VECTOR ( 'NONE', #10711, 1000.000000000000114 ) ;
#14627 = VECTOR ( 'NONE', #14738, 1000.000000000000114 ) ;
#14628 = PLANE ( 'NONE',  #11815 ) ;
#14629 = CARTESIAN_POINT ( 'NONE',  ( -1.144235203016679359, -3.958177651039096911, -0.09382832055446428676 ) ) ;
#14630 = DIRECTION ( 'NONE',  ( 0.000000000000000000, 0.000000000000000000, 1.000000000000000000 ) ) ;
#14631 = CARTESIAN_POINT ( 'NONE',  ( -8.190561711645485556E-16, -21.93750000136559208, 4.458734124999999437 ) ) ;
#14632 = FACE_BOUND ( 'NONE', #4902, .T. ) ;
#14633 = CIRCLE ( 'NONE', #12033, 75.00000000000001421 ) ;
#14634 = DIRECTION ( 'NONE',  ( 1.000000000000000000, 0.000000000000000000, 0.000000000000000000 ) ) ;
#14635 = CARTESIAN_POINT ( 'NONE',  ( 67.49999999999931788, 50.00000000000000000, 2.081668171172168513E-14 ) ) ;
#14636 = CARTESIAN_POINT ( 'NONE',  ( -2.390265326283148806, -4.391654775818394363, -6.249999997268814944 ) ) ;
#14637 = CYLINDRICAL_SURFACE ( 'NONE', #9241, 5.000000000000000000 ) ;
#14638 = CARTESIAN_POINT ( 'NONE',  ( -35.00000000000000000, 37.00000000000000000, -5.999999999999991118 ) ) ;
#14639 = ORIENTED_EDGE ( 'NONE', *, *, #14411, .T. ) ;
#14640 = DIRECTION ( 'NONE',  ( -0.000000000000000000, -1.000000000000000000, -0.000000000000000000 ) ) ;
#14641 = EDGE_LOOP ( 'NONE', ( #10218, #12041, #13692, #15327 ) ) ;
#14642 = CARTESIAN_POINT ( 'NONE',  ( -28.86751345948129455, -37.00000000000000711, 49.99999999999999289 ) ) ;
#14643 = EDGE_CURVE ( 'NONE', #7289, #12753, #6994, .T. ) ;
#14644 = ORIENTED_EDGE ( 'NONE', *, *, #7294, .F. ) ;
#14645 = VECTOR ( 'NONE', #6344, 1000.000000000000000 ) ;
#14646 = CARTESIAN_POINT ( 'NONE',  ( 19.99999999999956657, -8.786575603324269439E-13, -6.000000000000000000 ) ) ;
#14647 = CARTESIAN_POINT ( 'NONE',  ( -0.5711823568785977523, -5.381735091635034607, -4.187499997268818497 ) ) ;
#14648 = VECTOR ( 'NONE', #2107, 1000.000000000000000 ) ;
#14649 = CARTESIAN_POINT ( 'NONE',  ( 3.033343224707661712, -3.753672977998669946, 1.500000001365594304 ) ) ;
#14650 = CARTESIAN_POINT ( 'NONE',  ( -67.50000000000001421, 55.00000000000000000, -7.077671781985372945E-13 ) ) ;
#14651 = CARTESIAN_POINT ( 'NONE',  ( 4.276409079477644148, 1.261996585732577891, -2.562499998634407028 ) ) ;
#14652 = CARTESIAN_POINT ( 'NONE',  ( 0.000000000000000000, -32.00000000000000000, 0.000000000000000000 ) ) ;
#14653 = CIRCLE ( 'NONE', #7707, 2.649999999999985700 ) ;
#14654 = CARTESIAN_POINT ( 'NONE',  ( 2.071067811865476394, -22.31250000273118417, 5.000000000000000000 ) ) ;
#14655 = VERTEX_POINT ( 'NONE', #3111 ) ;
#14656 = CARTESIAN_POINT ( 'NONE',  ( -5.000000000000000000, -22.50000000000000000, -6.123233995736766282E-16 ) ) ;
#14657 = ORIENTED_EDGE ( 'NONE', *, *, #15794, .T. ) ;
#14658 = EDGE_LOOP ( 'NONE', ( #12043, #6592, #15319, #14150 ) ) ;
#14659 = ORIENTED_EDGE ( 'NONE', *, *, #13235, .F. ) ;
#14660 = CIRCLE ( 'NONE', #4600, 2.041999999999999815 ) ;
#14661 = ORIENTED_EDGE ( 'NONE', *, *, #10397, .T. ) ;
#14662 = CARTESIAN_POINT ( 'NONE',  ( -3.753672977998669502, -3.033343224707661712, -1.999999998634408360 ) ) ;
#14663 = LINE ( 'NONE', #14741, #7363 ) ;
#14664 = AXIS2_PLACEMENT_3D ( 'NONE', #13871, #2804, #15017 ) ;
#14665 = VECTOR ( 'NONE', #7469, 1000.000000000000114 ) ;
#14666 = CARTESIAN_POINT ( 'NONE',  ( -5.000000000000000888, -29.56250000000000355, -2.071067811865475949 ) ) ;
#14667 = CYLINDRICAL_SURFACE ( 'NONE', #14387, 57.99999999999999289 ) ;
#14668 = CARTESIAN_POINT ( 'NONE',  ( 5.000000000000004441, -2.247904837838113790E-16, -2.045263047592944528 ) ) ;
#14669 = DIRECTION ( 'NONE',  ( -0.000000000000000000, -1.000000000000000000, -0.000000000000000000 ) ) ;
#14670 = CONICAL_SURFACE ( 'NONE', #9768, 4.000000000000000000, 0.8911886515913786111 ) ;
#14671 = CARTESIAN_POINT ( 'NONE',  ( 5.381735091635035495, -0.5711823568785978633, 0.06250000273118166971 ) ) ;
#14672 = EDGE_CURVE ( 'NONE', #12016, #12678, #1147, .T. ) ;
#14673 =( NAMED_UNIT ( * ) PLANE_ANGLE_UNIT ( ) SI_UNIT ( $, .RADIAN. ) );
#14674 = CARTESIAN_POINT ( 'NONE',  ( 4.458734124999997661, -24.75000000136559564, 1.846868145590737864 ) ) ;
#14675 = CARTESIAN_POINT ( 'NONE',  ( -4.000000000000000000, -2.309401076758512694, -5.000000000000000000 ) ) ;
#14676 = CARTESIAN_POINT ( 'NONE',  ( -0.5093500532425060401, -4.799145180956616130, -3.624999998634407916 ) ) ;
#14677 = DIRECTION ( 'NONE',  ( 0.000000000000000000, 0.000000000000000000, -1.000000000000000000 ) ) ;
#14678 = VERTEX_POINT ( 'NONE', #5690 ) ;
#14679 = AXIS2_PLACEMENT_3D ( 'NONE', #7424, #4091, #5067 ) ;
#14680 = EDGE_LOOP ( 'NONE', ( #4659, #1039, #8300, #10921, #5319 ) ) ;
#14681 = AXIS2_PLACEMENT_3D ( 'NONE', #12351, #5172, #13641 ) ;
#14682 = DIRECTION ( 'NONE',  ( 0.000000000000000000, 0.000000000000000000, 1.000000000000000000 ) ) ;
#14683 = ORIENTED_EDGE ( 'NONE', *, *, #3307, .T. ) ;
#14684 = PRODUCT_DEFINITION_SHAPE ( 'NONE', 'NONE',  #15972 ) ;
#14685 = CARTESIAN_POINT ( 'NONE',  ( -4.458734125000000326, -24.25000000136559564, -1.846868145590735644 ) ) ;
#14686 = FACE_OUTER_BOUND ( 'NONE', #12574, .T. ) ;
#14687 = AXIS2_PLACEMENT_3D ( 'NONE', #10967, #3688, #3377 ) ;
#14688 = DIRECTION ( 'NONE',  ( 1.000000000000000000, 0.000000000000000000, 0.000000000000000000 ) ) ;
#14689 = DIRECTION ( 'NONE',  ( 0.000000000000000000, 1.000000000000000000, 0.000000000000000000 ) ) ;
#14690 = DIRECTION ( 'NONE',  ( -1.000000000000000000, 0.000000000000000000, 0.000000000000000000 ) ) ;
#14691 = DIRECTION ( 'NONE',  ( 0.000000000000000000, 0.000000000000000000, -1.000000000000000000 ) ) ;
#14692 = VECTOR ( 'NONE', #11489, 1000.000000000000000 ) ;
#14693 = CARTESIAN_POINT ( 'NONE',  ( -4.209348295687703967, -3.401574460001763001, -0.4375000000000013323 ) ) ;
#14694 = CARTESIAN_POINT ( 'NONE',  ( 2.500000000000000000, 2.357898499370433054, -1.951563910473907981E-15 ) ) ;
#14695 = ADVANCED_FACE ( 'NONE', ( #15398, #2345 ), #4322, .T. ) ;
#14696 = EDGE_CURVE ( 'NONE', #3133, #15535, #7112, .T. ) ;
#14697 = CARTESIAN_POINT ( 'NONE',  ( -1.846868145590737420, -27.75000000136559564, 4.458734124999999437 ) ) ;
#14698 = CARTESIAN_POINT ( 'NONE',  ( 0.5093500532425063732, 4.799145180956616130, -1.374999998634406140 ) ) ;
#14699 = EDGE_LOOP ( 'NONE', ( #15965, #12712 ) ) ;
#14700 = CARTESIAN_POINT ( 'NONE',  ( 23.49999999999956657, -8.782289339527253835E-13, 1.500000000000000000 ) ) ;
#14701 = EDGE_LOOP ( 'NONE', ( #7063, #14065, #4819, #5409 ) ) ;
#14702 = ORIENTED_EDGE ( 'NONE', *, *, #5522, .F. ) ;
#14703 = CARTESIAN_POINT ( 'NONE',  ( -94.14213562373093680, -97.39146311738100792, -17.50000000000000000 ) ) ;
#14704 = CARTESIAN_POINT ( 'NONE',  ( 4.458734125000000326, -25.37500000136559919, -1.846868145590734978 ) ) ;
#14705 = CARTESIAN_POINT ( 'NONE',  ( -21.01110699893060030, 0.000000000000000000, 33.74230484541324415 ) ) ;
#14706 = ORIENTED_EDGE ( 'NONE', *, *, #8108, .T. ) ;
#14707 = CARTESIAN_POINT ( 'NONE',  ( 0.000000000000000000, 40.00000000000000000, 0.000000000000000000 ) ) ;
#14708 =( BOUNDED_SURFACE ( )  B_SPLINE_SURFACE ( 3, 2, ( 
 ( #14410, #5601, #758 ),
 ( #3404, #830, #10618 ),
 ( #10769, #15706, #2186 ),
 ( #4464, #14322, #15473 ),
 ( #4625, #13247, #5752 ),
 ( #7139, #12042, #15623 ),
 ( #5521, #1952, #12936 ),
 ( #4307, #9248, #14174 ) ),
 .UNSPECIFIED., .F., .F., .F. ) 
 B_SPLINE_SURFACE_WITH_KNOTS ( ( 4, 2, 2, 4 ),
 ( 3, 3 ),
 ( 0.03861844051980969222, 0.04325213341840641879, 0.04556897986770477860, 0.04788582631700313841 ),
 ( 0.000000000000000000, 1.000000000000000000 ),
 .UNSPECIFIED. ) 
 GEOMETRIC_REPRESENTATION_ITEM ( )  RATIONAL_B_SPLINE_SURFACE ( (
 ( 1.000000000000000000, 0.8047781759831923454, 1.000000000000000000),
 ( 1.000000000000000000, 0.8123762462803808537, 1.000000000000000000),
 ( 1.000000000000000000, 0.8190659850618393634, 1.000000000000000000),
 ( 1.000000000000000000, 0.8191937571012808394, 1.000000000000000000),
 ( 1.000000000000000000, 0.8176092952779425715, 1.000000000000000000),
 ( 1.000000000000000000, 0.8122962088597516228, 1.000000000000000000),
 ( 1.000000000000000000, 0.8086311330827178345, 1.000000000000000000),
 ( 1.000000000000000000, 0.8047712282214325441, 1.000000000000000000) ) ) 
 REPRESENTATION_ITEM ( '' )  SURFACE ( )  );
#14709 = CARTESIAN_POINT ( 'NONE',  ( 2.500000000000000000, -1.178949249685213863, 2.042000000000002924 ) ) ;
#14710 = CARTESIAN_POINT ( 'NONE',  ( 4.101954839143060028, 2.368264730582927857, -3.681130640444267854 ) ) ;
#14711 = FACE_BOUND ( 'NONE', #6979, .T. ) ;
#14712 = CARTESIAN_POINT ( 'NONE',  ( -1.846868145590737420, -23.00000000136559564, 4.458734124999999437 ) ) ;
#14713 = CARTESIAN_POINT ( 'NONE',  ( 31.75426480542940766, -4.999999999999997335, 15.00000000000001243 ) ) ;
#14714 = EDGE_CURVE ( 'NONE', #6319, #362, #10555, .T. ) ;
#14715 = CARTESIAN_POINT ( 'NONE',  ( 4.999999999999849898, -1.272547481429012084, -0.9615974799134627826 ) ) ;
#14716 = ADVANCED_FACE ( 'NONE', ( #15483 ), #12237, .T. ) ;
#14717 = CARTESIAN_POINT ( 'NONE',  ( -3.535533905932737309, -29.75000000273118417, -3.535533905932738197 ) ) ;
#14718 = LINE ( 'NONE', #5095, #10416 ) ;
#14719 = DIRECTION ( 'NONE',  ( 0.000000000000000000, 1.000000000000000000, 0.000000000000000000 ) ) ;
#14720 = CARTESIAN_POINT ( 'NONE',  ( 5.000000000000000000, -25.06250000000000000, 2.071067811865478614 ) ) ;
#14721 = EDGE_LOOP ( 'NONE', ( #2586, #154, #4559, #10071 ) ) ;
#14722 = ORIENTED_EDGE ( 'NONE', *, *, #1114, .T. ) ;
#14723 = DIRECTION ( 'NONE',  ( -0.8306121863236411995, -0.2451191463975535001, -0.4999999999999953371 ) ) ;
#14724 = VERTEX_POINT ( 'NONE', #12192 ) ;
#14725 = DIRECTION ( 'NONE',  ( 1.000000000000000000, 0.000000000000000000, 0.000000000000000000 ) ) ;
#14726 = CARTESIAN_POINT ( 'NONE',  ( -4.211140560182196957, 2.431303136016537803, -3.745885042887433514 ) ) ;
#14727 = CARTESIAN_POINT ( 'NONE',  ( 3.753672977998667726, 3.033343224707664376, -2.249999998634408804 ) ) ;
#14728 = CARTESIAN_POINT ( 'NONE',  ( 67.49999999999931788, 32.00000000000000000, 2.081668171172168513E-14 ) ) ;
#14729 = EDGE_CURVE ( 'NONE', #9634, #2989, #13109, .T. ) ;
#14730 = CARTESIAN_POINT ( 'NONE',  ( -3.033343224707664376, 3.753672977998667726, -2.249999998634408804 ) ) ;
#14731 = FILL_AREA_STYLE_COLOUR ( '', #11299 ) ;
#14732 = MANIFOLD_SOLID_BREP ( 'EndChamfer', #3261 ) ;
#14733 = SHAPE_REPRESENTATION ( 'Circular Main Body Shell', ( #3223 ), #1673 ) ;
#14734 = CARTESIAN_POINT ( 'NONE',  ( 2.500000000000000000, -1.178949249685213863, 2.042000000000002924 ) ) ;
#14735 = CARTESIAN_POINT ( 'NONE',  ( 3.061616997868383141E-16, -22.75000000000000000, -4.999999999999999112 ) ) ;
#14736 = ORIENTED_EDGE ( 'NONE', *, *, #6179, .T. ) ;
#14737 = CARTESIAN_POINT ( 'NONE',  ( 6.000000000000000000, -20.00000000000000000, -1.500000000000000000 ) ) ;
#14738 = DIRECTION ( 'NONE',  ( 0.000000000000000000, -0.4999999999999993894, 0.8660254037844389297 ) ) ;
#14739 = ORIENTED_EDGE ( 'NONE', *, *, #3962, .F. ) ;
#14740 = CARTESIAN_POINT ( 'NONE',  ( -4.276409079477644148, -1.261996585732578335, -1.062499998634405696 ) ) ;
#14741 = CARTESIAN_POINT ( 'NONE',  ( 12.67949192431120586, -37.00000000000000711, 61.96152422706632024 ) ) ;
#14742 = CARTESIAN_POINT ( 'NONE',  ( 0.000000000000000000, -13.00000000000000178, -1.500000000000000000 ) ) ;
#14743 = DIRECTION ( 'NONE',  ( 0.000000000000000000, 0.000000000000000000, 1.000000000000000000 ) ) ;
#14744 = DIRECTION ( 'NONE',  ( 0.000000000000000000, 1.000000000000000000, 0.000000000000000000 ) ) ;
#14745 = EDGE_CURVE ( 'NONE', #5972, #9599, #1541, .T. ) ;
#14746 = CARTESIAN_POINT ( 'NONE',  ( 3.061616997868383141E-16, -30.87500000273118772, -5.000000000000000000 ) ) ;
#14747 = CARTESIAN_POINT ( 'NONE',  ( -1.415196051561583790, 4.795541693661363958, -1.624999997268814722 ) ) ;
#14748 = CARTESIAN_POINT ( 'NONE',  ( -41.99999999999978684, -9.000000000000001776, 3.499999999999998668 ) ) ;
#14749 = CARTESIAN_POINT ( 'NONE',  ( -4.458734124999999437, -24.25000000136559564, -1.846868145590735644 ) ) ;
#14750 = CARTESIAN_POINT ( 'NONE',  ( 4.458734124999999437, -23.43750000136559564, 0.000000000000000000 ) ) ;
#14751 = CARTESIAN_POINT ( 'NONE',  ( -3.033343224707664376, 3.753672977998667726, -2.999999998634409248 ) ) ;
#14752 = DIRECTION ( 'NONE',  ( 0.000000000000000000, 1.000000000000000000, -0.000000000000000000 ) ) ;
#14753 = VERTEX_POINT ( 'NONE', #6478 ) ;
#14754 = ORIENTED_EDGE ( 'NONE', *, *, #1732, .T. ) ;
#14755 = CIRCLE ( 'NONE', #3651, 2.649999999999992806 ) ;
#14756 = DIRECTION ( 'NONE',  ( 0.000000000000000000, 0.000000000000000000, 1.000000000000000000 ) ) ;
#14757 = ORIENTED_EDGE ( 'NONE', *, *, #15028, .F. ) ;
#14758 = CARTESIAN_POINT ( 'NONE',  ( -8.190561711645485556E-16, -22.93750000136559564, 4.458734124999999437 ) ) ;
#14759 = CARTESIAN_POINT ( 'NONE',  ( 0.000000000000000000, 37.00000000000000000, 0.000000000000000000 ) ) ;
#14760 = MANIFOLD_SOLID_BREP ( 'M5 Clearance Hole1', #10510 ) ;
#14761 = DIRECTION ( 'NONE',  ( 1.000000000000000000, 0.000000000000000000, 0.000000000000000000 ) ) ;
#14762 = EDGE_CURVE ( 'NONE', #6707, #7837, #7366, .T. ) ;
#14763 = B_SPLINE_CURVE_WITH_KNOTS ( 'NONE', 3,
 ( #6264, #9022, #11107, #11178, #8851, #2776 ),
 .UNSPECIFIED., .F., .F.,
 ( 4, 2, 4 ),
 ( 2.475503369425938985E-07, 0.002222330217055646252, 0.004444412883774351460 ),
 .UNSPECIFIED. ) ;
#14764 = FACE_OUTER_BOUND ( 'NONE', #8271, .T. ) ;
#14765 = CARTESIAN_POINT ( 'NONE',  ( -124.9999999999999716, -115.2072594216369339, 13.35786437626904366 ) ) ;
#14766 = CARTESIAN_POINT ( 'NONE',  ( 2.071067811865475505, -22.81250000000000000, -5.000000000000000888 ) ) ;
#14767 = CARTESIAN_POINT ( 'NONE',  ( 4.209348295687701302, 3.401574460001765665, 0.06249999999999536482 ) ) ;
#14768 = LINE ( 'NONE', #12244, #8870 ) ;
#14769 = DIRECTION ( 'NONE',  ( -0.8660254037844387076, 0.000000000000000000, 0.4999999999999997224 ) ) ;
#14770 = CARTESIAN_POINT ( 'NONE',  ( -1.846868145590734756, -27.12500000136559564, -4.458734125000000326 ) ) ;
#14771 = CARTESIAN_POINT ( 'NONE',  ( -4.276409079477644148, -1.261996585732578335, -4.062499998634405252 ) ) ;
#14772 = VERTEX_POINT ( 'NONE', #2742 ) ;
#14773 = DIRECTION ( 'NONE',  ( 0.000000000000000000, 0.000000000000000000, -1.000000000000000000 ) ) ;
#14774 = ORIENTED_EDGE ( 'NONE', *, *, #3492, .F. ) ;
#14775 = VERTEX_POINT ( 'NONE', #11391 ) ;
#14776 = DIRECTION ( 'NONE',  ( 0.000000000000000000, 1.000000000000000000, 0.000000000000000000 ) ) ;
#14777 = CARTESIAN_POINT ( 'NONE',  ( -1.846868145590734756, -23.12500000136559564, -4.458734125000000326 ) ) ;
#14778 = LINE ( 'NONE', #8571, #5045 ) ;
#14779 = ORIENTED_EDGE ( 'NONE', *, *, #5736, .F. ) ;
#14780 = DIRECTION ( 'NONE',  ( -0.000000000000000000, 0.000000000000000000, -1.000000000000000000 ) ) ;
#14781 = ADVANCED_FACE ( 'NONE', ( #8825 ), #19, .F. ) ;
#14782 = AXIS2_PLACEMENT_3D ( 'NONE', #237, #5155, #15012 ) ;
#14783 = ADVANCED_FACE ( 'NONE', ( #4936 ), #3715, .F. ) ;
#14784 = FACE_OUTER_BOUND ( 'NONE', #15544, .T. ) ;
#14785 = LINE ( 'NONE', #4765, #5632 ) ;
#14786 = DIRECTION ( 'NONE',  ( -0.000000000000000000, -1.000000000000000000, -0.000000000000000000 ) ) ;
#14787 = CARTESIAN_POINT ( 'NONE',  ( -4.458734125000001214, -24.12500000136559919, 1.846868145590734089 ) ) ;
#14788 = AXIS2_PLACEMENT_3D ( 'NONE', #5968, #15830, #1033 ) ;
#14789 = DIRECTION ( 'NONE',  ( 1.000000000000000000, 0.000000000000000000, 0.000000000000000000 ) ) ;
#14790 = CARTESIAN_POINT ( 'NONE',  ( 0.000000000000000000, 0.000000000000000000, -25.03750572909317285 ) ) ;
#14791 = CARTESIAN_POINT ( 'NONE',  ( 3.535533905932736864, -28.25000000273118772, 3.535533905932738641 ) ) ;
#14792 = CARTESIAN_POINT ( 'NONE',  ( 30.02221399786053979, 0.000000000000000000, -15.99999999999998579 ) ) ;
#14793 = VECTOR ( 'NONE', #8744, 1000.000000000000000 ) ;
#14794 = CARTESIAN_POINT ( 'NONE',  ( 3.061616997868383141E-16, -23.87500000273118772, -5.000000000000000000 ) ) ;
#14795 = CARTESIAN_POINT ( 'NONE',  ( 2.500000000000000000, -1.178949249685218303, -2.041999999999998039 ) ) ;
#14796 = EDGE_LOOP ( 'NONE', ( #11432, #13954, #2745, #5893 ) ) ;
#14797 = EDGE_LOOP ( 'NONE', ( #6658, #15771, #433, #5602 ) ) ;
#14798 = CARTESIAN_POINT ( 'NONE',  ( 2.500000000000000000, 0.000000000000000000, 2.041999999999999815 ) ) ;
#14799 =( BOUNDED_CURVE ( )  B_SPLINE_CURVE ( 2, ( #341, #7698, #9861, #8746, #5181, #10109, #3800, #6396, #14794 ),
 .UNSPECIFIED., .F., .F. ) 
 B_SPLINE_CURVE_WITH_KNOTS ( ( 3, 2, 2, 2, 3 ),
 ( 0.6749999999999999334, 0.6874999999999998890, 0.6999999999999999556, 0.7125000000000000222, 0.7249999999999999778 ),
 .UNSPECIFIED. ) 
 CURVE ( )  GEOMETRIC_REPRESENTATION_ITEM ( )  RATIONAL_B_SPLINE_CURVE ( ( 1.000000000000000666, 0.9238795325112860723, 1.000000000000000000, 0.9238795325112867385, 1.000000000000000000, 0.9238795325112867385, 1.000000000000000000, 0.9238795325112867385, 1.000000000000000000 ) ) 
 REPRESENTATION_ITEM ( '' )  );
#14800 = ORIENTED_EDGE ( 'NONE', *, *, #3480, .F. ) ;
#14801 = VECTOR ( 'NONE', #1104, 1000.000000000000000 ) ;
#14802 = CYLINDRICAL_SURFACE ( 'NONE', #11514, 5.000000000000000888 ) ;
#14803 = EDGE_CURVE ( 'NONE', #2119, #7795, #13726, .T. ) ;
#14804 = CARTESIAN_POINT ( 'NONE',  ( 3.061616997868383141E-16, -25.87500000273118417, -5.000000000000000000 ) ) ;
#14805 = CARTESIAN_POINT ( 'NONE',  ( 3.753672977998667726, 3.033343224707664376, -3.249999998634409692 ) ) ;
#14806 = SHAPE_DEFINITION_REPRESENTATION ( #12846, #9778 ) ;
#14807 = CARTESIAN_POINT ( 'NONE',  ( -1.261996585732579224, 4.276409079477648589, -4.312499998634405252 ) ) ;
#14808 =( NAMED_UNIT ( * ) PLANE_ANGLE_UNIT ( ) SI_UNIT ( $, .RADIAN. ) );
#14809 = CYLINDRICAL_SURFACE ( 'NONE', #10550, 5.000000000000000000 ) ;
#14810 = CARTESIAN_POINT ( 'NONE',  ( 23.49999999999956657, -8.786575603324269439E-13, -13.00000000000000000 ) ) ;
#14811 = VERTEX_POINT ( 'NONE', #6238 ) ;
#14812 = DIRECTION ( 'NONE',  ( 0.8660254037844383745, 0.000000000000000000, 0.5000000000000006661 ) ) ;
#14813 = EDGE_LOOP ( 'NONE', ( #7308, #7785 ) ) ;
#14814 = EDGE_LOOP ( 'NONE', ( #2093, #15048 ) ) ;
#14815 = CONTEXT_DEPENDENT_SHAPE_REPRESENTATION ( #10542, #6641 ) ;
#14816 = CARTESIAN_POINT ( 'NONE',  ( 4.799145180956616130, -0.5093500532425063732, -4.624999998634405252 ) ) ;
#14817 = EDGE_CURVE ( 'NONE', #8388, #8643, #3485, .T. ) ;
#14818 = EDGE_CURVE ( 'NONE', #4993, #7943, #1369, .T. ) ;
#14819 = EDGE_CURVE ( 'NONE', #635, #5764, #2505, .T. ) ;
#14820 = VECTOR ( 'NONE', #9301, 1000.000000000000000 ) ;
#14821 = DIRECTION ( 'NONE',  ( 0.000000000000000000, 0.000000000000000000, 1.000000000000000000 ) ) ;
#14822 = CARTESIAN_POINT ( 'NONE',  ( -2.855764796983342624, 2.970025579236414082, -0.09382832055445475272 ) ) ;
#14823 = CARTESIAN_POINT ( 'NONE',  ( 67.49999999999931788, 40.00000000000000000, -2.649999999999971934 ) ) ;
#14824 = LINE ( 'NONE', #15298, #10886 ) ;
#14825 = UNCERTAINTY_MEASURE_WITH_UNIT (LENGTH_MEASURE( 1.000000000000000082E-05 ), #4462, 'distance_accuracy_value', 'NONE');
#14826 = CARTESIAN_POINT ( 'NONE',  ( 6.000000000000000000, -13.00000000000000178, 1.500000000000000000 ) ) ;
#14827 = AXIS2_PLACEMENT_3D ( 'NONE', #14489, #3342, #9560 ) ;
#14828 = CARTESIAN_POINT ( 'NONE',  ( 1.415196051561583790, -4.795541693661363958, -3.124999997268815832 ) ) ;
#14829 = DIRECTION ( 'NONE',  ( 1.000000000000000000, 0.000000000000000000, 0.000000000000000000 ) ) ;
#14830 = CARTESIAN_POINT ( 'NONE',  ( -4.619058391327882873, 0.6486937841448088271, -0.2428057022536735388 ) ) ;
#14831 = CARTESIAN_POINT ( 'NONE',  ( -1.846868145590734756, -26.37500000136559564, -4.458734124999999437 ) ) ;
#14832 = VERTEX_POINT ( 'NONE', #6793 ) ;
#14833 = AXIS2_PLACEMENT_3D ( 'NONE', #1896, #14111, #15411 ) ;
#14834 = CARTESIAN_POINT ( 'NONE',  ( -3.152801135295367096, -24.06250000136559564, -3.152801135295367541 ) ) ;
#14835 = CARTESIAN_POINT ( 'NONE',  ( -0.5093500532425060401, -4.799145180956616130, -4.624999998634405252 ) ) ;
#14836 = CARTESIAN_POINT ( 'NONE',  ( 35.00000000000000000, 40.00000000000000000, 5.999999999999991118 ) ) ;
#14837 = ORIENTED_EDGE ( 'NONE', *, *, #14714, .T. ) ;
#14838 = ORIENTED_EDGE ( 'NONE', *, *, #11102, .T. ) ;
#14839 = DIRECTION ( 'NONE',  ( 1.000000000000000000, 0.000000000000000000, 0.000000000000000000 ) ) ;
#14840 = ORIENTED_EDGE ( 'NONE', *, *, #688, .T. ) ;
#14841 = CARTESIAN_POINT ( 'NONE',  ( 1.846868145590735200, -24.50000000136559564, -4.458734125000000326 ) ) ;
#14842 = CARTESIAN_POINT ( 'NONE',  ( 0.000000000000000000, -13.00000000000000178, 0.000000000000000000 ) ) ;
#14843 = AXIS2_PLACEMENT_3D ( 'NONE', #4078, #6758, #5381 ) ;
#14844 = EDGE_CURVE ( 'NONE', #10782, #14017, #11469, .T. ) ;
#14845 = CIRCLE ( 'NONE', #1417, 2.649999999999985700 ) ;
#14846 = LINE ( 'NONE', #4666, #10195 ) ;
#14847 = CARTESIAN_POINT ( 'NONE',  ( -7.922281120364393914, -4.573931137438277617, -8.047472243342932430 ) ) ;
#14848 = CARTESIAN_POINT ( 'NONE',  ( 0.000000000000000000, -13.00000000000000178, 0.000000000000000000 ) ) ;
#14849 = DIRECTION ( 'NONE',  ( -0.000000000000000000, -0.000000000000000000, -1.000000000000000000 ) ) ;
#14850 = CARTESIAN_POINT ( 'NONE',  ( 2.390265326283148806, 4.391654775818395251, -0.8750000000000007772 ) ) ;
#14851 = CARTESIAN_POINT ( 'NONE',  ( -4.391654775818395251, 2.390265326283148806, -3.624999999999999556 ) ) ;
#14852 = DIRECTION ( 'NONE',  ( 1.000000000000000000, 0.000000000000000000, 0.000000000000000000 ) ) ;
#14853 = CARTESIAN_POINT ( 'NONE',  ( -1.846868145590737420, -25.75000000136559564, 4.458734124999999437 ) ) ;
#14854 = CARTESIAN_POINT ( 'NONE',  ( -4.276409079477644148, -1.261996585732578335, -1.062499998634405696 ) ) ;
#14855 = ORIENTED_EDGE ( 'NONE', *, *, #10899, .T. ) ;
#14856 = AXIS2_PLACEMENT_3D ( 'NONE', #6554, #5498, #2903 ) ;
#14857 = CARTESIAN_POINT ( 'NONE',  ( -7.500000000000007105, -2.571118828324944428, -0.3627527587569141510 ) ) ;
#14858 = ORIENTED_EDGE ( 'NONE', *, *, #12740, .F. ) ;
#14859 = ORIENTED_EDGE ( 'NONE', *, *, #5097, .F. ) ;
#14861 = CARTESIAN_POINT ( 'NONE',  ( -67.50000000000000000, 40.00000000000000000, -2.650000000000699352 ) ) ;
#14860 = AXIS2_PLACEMENT_3D ( 'NONE', #10522, #4603, #6799 ) ;
#14862 = CARTESIAN_POINT ( 'NONE',  ( 4.458734124999999437, -25.43750000136559564, 0.000000000000000000 ) ) ;
#14863 = LINE ( 'NONE', #1600, #15914 ) ;
#14864 = VERTEX_POINT ( 'NONE', #8987 ) ;
#14865 = CARTESIAN_POINT ( 'NONE',  ( 0.000000000000000000, 0.000000000000000000, 0.000000000000000000 ) ) ;
#14866 = AXIS2_PLACEMENT_3D ( 'NONE', #15323, #7892, #1731 ) ;
#14867 = CARTESIAN_POINT ( 'NONE',  ( 6.601567268551446155, -5.319966374295976408, -7.792327460285857654 ) ) ;
#14868 = CYLINDRICAL_SURFACE ( 'NONE', #12325, 5.000000000000000888 ) ;
#14869 = DIRECTION ( 'NONE',  ( 0.000000000000000000, -0.000000000000000000, 1.000000000000000000 ) ) ;
#14870 = AXIS2_PLACEMENT_3D ( 'NONE', #13287, #10958, #9589 ) ;
#14871 = CARTESIAN_POINT ( 'NONE',  ( -5.000000000000000888, -28.56250000000000000, -2.071067811865475949 ) ) ;
#14872 = DIRECTION ( 'NONE',  ( -1.000000000000000000, 0.000000000000000000, 0.000000000000000000 ) ) ;
#14873 = APPLICATION_CONTEXT ( 'automotive_design' ) ;
#14874 = CARTESIAN_POINT ( 'NONE',  ( 1.567478505476134606E-15, 4.618802153517012066, -3.433295621305382905 ) ) ;
#14875 = CARTESIAN_POINT ( 'NONE',  ( 5.000000000000000000, -29.12500000273118772, 0.000000000000000000 ) ) ;
#14876 = CARTESIAN_POINT ( 'NONE',  ( -4.336808689942017736E-16, 9.147862274876558786, -8.047472243342932430 ) ) ;
#14877 = CARTESIAN_POINT ( 'NONE',  ( -4.458734125000000326, -29.87500000136559564, 1.846868145590734089 ) ) ;
#14878 = ADVANCED_FACE ( 'NONE', ( #7937, #15208 ), #6879, .F. ) ;
#14879 = CIRCLE ( 'NONE', #3271, 4.250000000000000000 ) ;
#14880 = VERTEX_POINT ( 'NONE', #5341 ) ;
#14881 =( GEOMETRIC_REPRESENTATION_CONTEXT ( 3 ) GLOBAL_UNCERTAINTY_ASSIGNED_CONTEXT ( ( #14994 ) ) GLOBAL_UNIT_ASSIGNED_CONTEXT ( ( #1475, #10128, #200 ) ) REPRESENTATION_CONTEXT ( 'NONE', 'WORKASPACE' ) );
#14882 =( LENGTH_UNIT ( ) NAMED_UNIT ( * ) SI_UNIT ( .MILLI., .METRE. ) );
#14883 = EDGE_LOOP ( 'NONE', ( #10430, #9357 ) ) ;
#14884 = CARTESIAN_POINT ( 'NONE',  ( 3.349226789952652439, 2.685125164760731487, -0.2236248678334773199 ) ) ;
#14885 = AXIS2_PLACEMENT_3D ( 'NONE', #13613, #11122, #3923 ) ;
#14886 = ORIENTED_EDGE ( 'NONE', *, *, #15093, .F. ) ;
#14887 = CIRCLE ( 'NONE', #10755, 2.499999999999998668 ) ;
#14888 = LINE ( 'NONE', #13567, #1459 ) ;
#14889 = TOROIDAL_SURFACE ( 'NONE', #2230, 4.000000000000000000, 0.2500000000000000000 ) ;
#14890 = CARTESIAN_POINT ( 'NONE',  ( 39.84679848243397515, -3.763931520638774675, 28.17238874121806091 ) ) ;
#14891 = CARTESIAN_POINT ( 'NONE',  ( 3.753672977998667726, 3.033343224707664376, -4.249999998634406140 ) ) ;
#14892 = DIRECTION ( 'NONE',  ( 0.000000000000000000, 0.000000000000000000, 1.000000000000000000 ) ) ;
#14893 = DIRECTION ( 'NONE',  ( -0.5000000000000041078, -6.123233995736766036E-17, -0.8660254037844364872 ) ) ;
#14894 = AXIS2_PLACEMENT_3D ( 'NONE', #4294, #4606, #14395 ) ;
#14895 = CARTESIAN_POINT ( 'NONE',  ( 4.799145180956616130, -0.5093500532425063732, -4.624999998634405252 ) ) ;
#14896 = CARTESIAN_POINT ( 'NONE',  ( 17.99999999999957012, -8.784126309725975241E-13, 0.000000000000000000 ) ) ;
#14897 = EDGE_CURVE ( 'NONE', #12880, #9400, #11783, .T. ) ;
#14898 = CARTESIAN_POINT ( 'NONE',  ( 27.50000000000003197, -5.000000000000000000, -47.63139720814412925 ) ) ;
#14900 = EDGE_CURVE ( 'NONE', #12212, #12835, #10477, .T. ) ;
#14899 = VERTEX_POINT ( 'NONE', #1779 ) ;
#14901 =( BOUNDED_CURVE ( )  B_SPLINE_CURVE ( 2, ( #13760, #12704, #2694, #6349, #5209, #4150, #9096, #6509, #10144 ),
 .UNSPECIFIED., .F., .F. ) 
 B_SPLINE_CURVE_WITH_KNOTS ( ( 3, 2, 2, 2, 3 ),
 ( 0.8250000000000000666, 0.8375000000000001332, 0.8500000000000000888, 0.8625000000000000444, 0.8750000000000000000 ),
 .UNSPECIFIED. ) 
 CURVE ( )  GEOMETRIC_REPRESENTATION_ITEM ( )  RATIONAL_B_SPLINE_CURVE ( ( 0.9999999999999993339, 0.9238795325112874046, 1.000000000000000000, 0.9238795325112867385, 1.000000000000000000, 0.9238795325112867385, 1.000000000000000000, 0.9238795325112867385, 1.000000000000000000 ) ) 
 REPRESENTATION_ITEM ( '' )  );
#14902 = CARTESIAN_POINT ( 'NONE',  ( 0.000000000000000000, -20.00000000000000000, 0.000000000000000000 ) ) ;
#14903 = ORIENTED_EDGE ( 'NONE', *, *, #6240, .F. ) ;
#14904 = FACE_OUTER_BOUND ( 'NONE', #9207, .T. ) ;
#14905 = AXIS2_PLACEMENT_3D ( 'NONE', #9257, #11813, #5609 ) ;
#14906 = CARTESIAN_POINT ( 'NONE',  ( 0.000000000000000000, 0.000000000000000000, 0.000000000000000000 ) ) ;
#14907 = EDGE_LOOP ( 'NONE', ( #6051, #4038, #3391, #2174 ) ) ;
#14908 = ITEM_DEFINED_TRANSFORMATION ( 'NONE', 'NONE', #8645,  #3223 ) ;
#14909 = CARTESIAN_POINT ( 'NONE',  ( -4.799145180956616130, 0.5093500532425063732, -6.124999998634407916 ) ) ;
#14910 = CARTESIAN_POINT ( 'NONE',  ( 4.000000000000000888, 1.563622288139206118, -0.2253451193528334950 ) ) ;
#14911 = CARTESIAN_POINT ( 'NONE',  ( -2.131511515620587272, -3.916244202832140253, -7.687499998634407916 ) ) ;
#14912 = VECTOR ( 'NONE', #12592, 1000.000000000000000 ) ;
#14913 = FACE_OUTER_BOUND ( 'NONE', #1784, .T. ) ;
#14914 = CARTESIAN_POINT ( 'NONE',  ( -1.999999999999999556, 3.464101615137754830, -3.142992957459232795 ) ) ;
#14915 = CARTESIAN_POINT ( 'NONE',  ( 4.795541693661363958, 1.415196051561583790, -4.874999997268817609 ) ) ;
#14916 = PLANE ( 'NONE',  #6818 ) ;
#14917 = EDGE_CURVE ( 'NONE', #11894, #12917, #3077, .T. ) ;
#14918 = CARTESIAN_POINT ( 'NONE',  ( 2.071067811865462183, -28.31250000273118772, 5.000000000000013323 ) ) ;
#14919 = CARTESIAN_POINT ( 'NONE',  ( -4.458734124999999437, -27.18750000136559564, -5.460374474430324690E-16 ) ) ;
#14920 = EDGE_CURVE ( 'NONE', #13455, #14678, #7899, .T. ) ;
#14921 = ORIENTED_EDGE ( 'NONE', *, *, #12795, .T. ) ;
#14922 = CARTESIAN_POINT ( 'NONE',  ( -21.01110699893041556, -1.230770033143087371E-15, -36.39230484541334221 ) ) ;
#14923 = CARTESIAN_POINT ( 'NONE',  ( 4.799145180956616130, -0.5093500532425063732, -2.374999998634407028 ) ) ;
#14924 = AXIS2_PLACEMENT_3D ( 'NONE', #5916, #7132, #9785 ) ;
#14925 = DIRECTION ( 'NONE',  ( 1.000000000000000000, 1.541976423090495140E-16, -0.000000000000000000 ) ) ;
#14926 = ORIENTED_EDGE ( 'NONE', *, *, #6676, .F. ) ;
#14927 = ORIENTED_EDGE ( 'NONE', *, *, #4623, .F. ) ;
#14928 = ORIENTED_EDGE ( 'NONE', *, *, #2217, .T. ) ;
#14929 = CARTESIAN_POINT ( 'NONE',  ( 1.846868145590736310, -23.87500000136559564, 4.458734124999999437 ) ) ;
#14930 = CONICAL_SURFACE ( 'NONE', #15954, 2.500000000000000888, 0.9599310885968785900 ) ;
#14931 = DIRECTION ( 'NONE',  ( -0.000000000000000000, 1.000000000000000000, -0.000000000000000000 ) ) ;
#14932 = AXIS2_PLACEMENT_3D ( 'NONE', #6350, #11269, #15069 ) ;
#14933 = CYLINDRICAL_SURFACE ( 'NONE', #10708, 2.649999999999992806 ) ;
#14934 = VECTOR ( 'NONE', #4878, 1000.000000000000000 ) ;
#14935 = CARTESIAN_POINT ( 'NONE',  ( 3.061616997868383141E-16, -25.75000000000000355, -5.000000000000000000 ) ) ;
#14936 = LINE ( 'NONE', #2875, #6529 ) ;
#14937 = FACE_OUTER_BOUND ( 'NONE', #8600, .T. ) ;
#14938 = CARTESIAN_POINT ( 'NONE',  ( 4.391654775818395251, -2.390265326283149694, -6.125000000000001776 ) ) ;
#14939 = CARTESIAN_POINT ( 'NONE',  ( 2.500000000000000000, 2.357898499370433054, -1.951563910473907981E-15 ) ) ;
#14940 = CIRCLE ( 'NONE', #15716, 5.000000000000000000 ) ;
#14941 = CARTESIAN_POINT ( 'NONE',  ( 0.1410422978106145031, -4.700232962125109104, -3.687027686973628704 ) ) ;
#14942 = CARTESIAN_POINT ( 'NONE',  ( 2.730187237215162345E-16, -26.18750000136559564, -4.458734124999999437 ) ) ;
#14943 = VECTOR ( 'NONE', #2094, 1000.000000000000000 ) ;
#14944 = EDGE_CURVE ( 'NONE', #10748, #10008, #4276, .T. ) ;
#14945 = CARTESIAN_POINT ( 'NONE',  ( 1.261996585732578113, -4.276409079477644148, -1.812499998634406584 ) ) ;
#14946 = ORIENTED_EDGE ( 'NONE', *, *, #3783, .T. ) ;
#14947 = DIRECTION ( 'NONE',  ( -0.000000000000000000, -0.000000000000000000, -1.000000000000000000 ) ) ;
#14948 = EDGE_LOOP ( 'NONE', ( #3434, #10079, #3802, #12971 ) ) ;
#14949 = ORIENTED_EDGE ( 'NONE', *, *, #1440, .F. ) ;
#14950 = AXIS2_PLACEMENT_3D ( 'NONE', #3671, #2531, #8384 ) ;
#14951 = LINE ( 'NONE', #14015, #9035 ) ;
#14952 = CARTESIAN_POINT ( 'NONE',  ( -3.152801135295367096, -24.06250000136559564, -3.152801135295367541 ) ) ;
#14953 = DIRECTION ( 'NONE',  ( 0.000000000000000000, 0.000000000000000000, -1.000000000000000000 ) ) ;
#14954 = VERTEX_POINT ( 'NONE', #6726 ) ;
#14955 = CARTESIAN_POINT ( 'NONE',  ( 1.360585162435110629, -4.061296242128317857, -3.505054077164905024 ) ) ;
#14956 = AXIS2_PLACEMENT_3D ( 'NONE', #8741, #3797, #12034 ) ;
#14957 = VECTOR ( 'NONE', #8414, 1000.000000000000000 ) ;
#14958 = CARTESIAN_POINT ( 'NONE',  ( 1.567478505476134606E-15, 4.618802153517012066, -5.000000000000000000 ) ) ;
#14959 = CARTESIAN_POINT ( 'NONE',  ( 4.276409079477644148, 1.261996585732577891, -3.312499998634407916 ) ) ;
#14960 = CARTESIAN_POINT ( 'NONE',  ( 4.078246330773204420, 1.822159612333905887, -0.3789984458506753806 ) ) ;
#14961 = CARTESIAN_POINT ( 'NONE',  ( -2.071067811865475061, -28.68750000000000711, -5.000000000000000888 ) ) ;
#14962 = DIRECTION ( 'NONE',  ( 0.000000000000000000, -0.000000000000000000, 1.000000000000000000 ) ) ;
#14963 = CARTESIAN_POINT ( 'NONE',  ( -90.00000000000000000, -95.00000000000000000, 7.500000000000001776 ) ) ;
#14964 = CARTESIAN_POINT ( 'NONE',  ( 5.000000000000000000, -28.18750000273119127, 2.071067811865478614 ) ) ;
#14965 = ADVANCED_FACE ( 'NONE', ( #4121 ), #4175, .F. ) ;
#14966 = CARTESIAN_POINT ( 'NONE',  ( 0.000000000000000000, -13.00000000000000178, 1.500000000000000000 ) ) ;
#14967 = CARTESIAN_POINT ( 'NONE',  ( -1.846868145590734756, -30.12500000136559564, -4.458734124999999437 ) ) ;
#14968 = ORIENTED_EDGE ( 'NONE', *, *, #2589, .T. ) ;
#14969 = ORIENTED_EDGE ( 'NONE', *, *, #11945, .F. ) ;
#14970 = CIRCLE ( 'NONE', #2308, 9.999999999999994671 ) ;
#14971 = VERTEX_POINT ( 'NONE', #3534 ) ;
#14972 = DIRECTION ( 'NONE',  ( -0.8660254037844383745, 0.000000000000000000, -0.5000000000000004441 ) ) ;
#14973 = ORIENTED_EDGE ( 'NONE', *, *, #2365, .F. ) ;
#14974 = DIRECTION ( 'NONE',  ( 0.000000000000000000, 0.000000000000000000, 1.000000000000000000 ) ) ;
#14975 = APPLICATION_CONTEXT ( 'automotive_design' ) ;
#14976 = EDGE_CURVE ( 'NONE', #2457, #9104, #1157, .T. ) ;
#14977 = CARTESIAN_POINT ( 'NONE',  ( -3.152801135295367985, -31.06250000136559564, 3.152801135295367096 ) ) ;
#14978 = SHAPE_DEFINITION_REPRESENTATION ( #10411, #396 ) ;
#14979 = CARTESIAN_POINT ( 'NONE',  ( 3.753672977998667726, 3.033343224707664376, -4.499999998634407028 ) ) ;
#14980 = CARTESIAN_POINT ( 'NONE',  ( 21.99999999999956657, -8.786575603324269439E-13, -11.50000000000000000 ) ) ;
#14981 = LINE ( 'NONE', #9804, #15718 ) ;
#14982 = ORIENTED_EDGE ( 'NONE', *, *, #7751, .T. ) ;
#14983 = CARTESIAN_POINT ( 'NONE',  ( 2.500000000000000000, -1.178949249685213863, 2.042000000000002924 ) ) ;
#14984 = ORIENTED_EDGE ( 'NONE', *, *, #14729, .T. ) ;
#14985 = CARTESIAN_POINT ( 'NONE',  ( 5.000000000000004441, -2.247904837838113790E-16, -7.045263047592947636 ) ) ;
#14986 = DIRECTION ( 'NONE',  ( 0.000000000000000000, 1.000000000000000000, 0.000000000000000000 ) ) ;
#14987 = ORIENTED_EDGE ( 'NONE', *, *, #5391, .F. ) ;
#14988 = CARTESIAN_POINT ( 'NONE',  ( 4.276409079477644148, 1.261996585732577891, -5.562499998634406140 ) ) ;
#14989 = DIRECTION ( 'NONE',  ( 1.000000000000000000, 0.000000000000000000, 0.000000000000000000 ) ) ;
#14990 = EDGE_CURVE ( 'NONE', #14592, #9703, #9188, .T. ) ;
#14991 = EDGE_CURVE ( 'NONE', #8828, #12259, #5573, .T. ) ;
#14992 = CARTESIAN_POINT ( 'NONE',  ( -2.071067811865457742, -28.81250000273119127, -5.000000000000019540 ) ) ;
#14993 = DIRECTION ( 'NONE',  ( -0.5000000000000002220, 0.000000000000000000, 0.8660254037844385966 ) ) ;
#14994 = UNCERTAINTY_MEASURE_WITH_UNIT (LENGTH_MEASURE( 1.000000000000000082E-05 ), #1475, 'distance_accuracy_value', 'NONE');
#14995 = CARTESIAN_POINT ( 'NONE',  ( 3.061616997868383141E-16, -26.87500000273118772, -5.000000000000000000 ) ) ;
#14996 = CARTESIAN_POINT ( 'NONE',  ( -5.381735091635034607, 0.5711823568785950878, -5.437499997268815832 ) ) ;
#14997 = CARTESIAN_POINT ( 'NONE',  ( -7.922281120364393914, 4.573931137438272287, -8.047472243342932430 ) ) ;
#14998 = CARTESIAN_POINT ( 'NONE',  ( -2.799455000695346918, 3.610413774745345528, -0.3100886528999980407 ) ) ;
#14999 = DIRECTION ( 'NONE',  ( 0.000000000000000000, -1.000000000000000000, 0.000000000000000000 ) ) ;
#15000 = VERTEX_POINT ( 'NONE', #2326 ) ;
#15001 = FACE_OUTER_BOUND ( 'NONE', #4124, .T. ) ;
#15002 = CARTESIAN_POINT ( 'NONE',  ( -28.86751345948130165, 0.000000000000000000, 18.00000000000000355 ) ) ;
#15003 = CARTESIAN_POINT ( 'NONE',  ( -28.86751345948196601, 0.000000000000000000, -75.00199999999976797 ) ) ;
#15004 = ORIENTED_EDGE ( 'NONE', *, *, #8308, .T. ) ;
#15005 = ORIENTED_EDGE ( 'NONE', *, *, #4488, .F. ) ;
#15006 = VERTEX_POINT ( 'NONE', #1110 ) ;
#15007 = FACE_OUTER_BOUND ( 'NONE', #3321, .T. ) ;
#15008 = CARTESIAN_POINT ( 'NONE',  ( -45.00000000000000711, -1.734723475976807094E-15, -13.35786437626904721 ) ) ;
#15009 = CARTESIAN_POINT ( 'NONE',  ( -2.886751345948099789, -37.00000000000000711, -35.00000000000000000 ) ) ;
#15010 = ADVANCED_FACE ( 'NONE', ( #12099 ), #13284, .F. ) ;
#15011 = CARTESIAN_POINT ( 'NONE',  ( 2.071067811865490160, -25.81250000000000355, -4.999999999999985789 ) ) ;
#15012 = DIRECTION ( 'NONE',  ( 0.000000000000000000, 0.000000000000000000, 1.000000000000000000 ) ) ;
#15013 = DIRECTION ( 'NONE',  ( -0.000000000000000000, 1.000000000000000000, -0.000000000000000000 ) ) ;
#15014 = PRODUCT_DEFINITION_SHAPE ( 'NONE', 'NONE',  #15993 ) ;
#15015 = CARTESIAN_POINT ( 'NONE',  ( 0.5711823568785989735, 5.381735091635026613, -6.812500000000005329 ) ) ;
#15016 = CARTESIAN_POINT ( 'NONE',  ( -44.99999999999997868, -34.99999999999999289, -13.35786437626904544 ) ) ;
#15017 = DIRECTION ( 'NONE',  ( 1.000000000000000000, 0.000000000000000000, 0.000000000000000000 ) ) ;
#15018 = CARTESIAN_POINT ( 'NONE',  ( -4.458734125000001214, -26.87500000136559208, 1.846868145590734089 ) ) ;
#15019 = CARTESIAN_POINT ( 'NONE',  ( 4.799145180956616130, -0.5093500532425063732, -4.624999998634405252 ) ) ;
#15020 = VERTEX_POINT ( 'NONE', #7198 ) ;
#15021 = CARTESIAN_POINT ( 'NONE',  ( -17.99999999999979394, -11.00000000000000178, -1.500000000000000888 ) ) ;
#15022 = ORIENTED_EDGE ( 'NONE', *, *, #6324, .F. ) ;
#15023 = EDGE_LOOP ( 'NONE', ( #10318, #5855, #5876, #4579 ) ) ;
#15024 = CARTESIAN_POINT ( 'NONE',  ( -4.458734125000001214, -21.87500000136559208, 1.846868145590734089 ) ) ;
#15025 = DIRECTION ( 'NONE',  ( -0.7071067811865369146, 0.000000000000000000, 0.7071067811865582309 ) ) ;
#15026 = EDGE_LOOP ( 'NONE', ( #12280, #11135, #1867, #1111 ) ) ;
#15027 = DIRECTION ( 'NONE',  ( 0.000000000000000000, 0.000000000000000000, 1.000000000000000000 ) ) ;
#15028 = EDGE_CURVE ( 'NONE', #15784, #10748, #7270, .T. ) ;
#15029 = AXIS2_PLACEMENT_3D ( 'NONE', #7398, #14640, #4890 ) ;
#15030 = ADVANCED_FACE ( 'NONE', ( #4519, #5731, #4444, #2164, #13388 ), #3227, .F. ) ;
#15031 = ADVANCED_FACE ( 'NONE', ( #8491 ), #10824, .F. ) ;
#15032 = ADVANCED_FACE ( 'NONE', ( #2014 ), #889, .T. ) ;
#15033 = DIRECTION ( 'NONE',  ( 0.000000000000000000, 0.000000000000000000, -1.000000000000000000 ) ) ;
#15034 = CARTESIAN_POINT ( 'NONE',  ( -3.753672977998669502, -3.033343224707661712, -1.749999998634408360 ) ) ;
#15035 = CARTESIAN_POINT ( 'NONE',  ( 4.434540660362028319, 0.5348740976411813230, -0.3789984458506921450 ) ) ;
#15036 = CARTESIAN_POINT ( 'NONE',  ( -5.000000000000000888, -28.43750000000000355, 2.071067811865474617 ) ) ;
#15037 = CYLINDRICAL_SURFACE ( 'NONE', #7089, 9.999999999999994671 ) ;
#15038 = FACE_OUTER_BOUND ( 'NONE', #14538, .T. ) ;
#15039 = CARTESIAN_POINT ( 'NONE',  ( -5.000000000000000000, -27.62500000273118772, -6.123233995736766282E-16 ) ) ;
#15040 = DIRECTION ( 'NONE',  ( 0.000000000000000000, 0.000000000000000000, 1.000000000000000000 ) ) ;
#15041 = CARTESIAN_POINT ( 'NONE',  ( -3.152801135295367096, -29.06250000136559564, -3.152801135295367541 ) ) ;
#15042 = SURFACE_SIDE_STYLE ('',( #10192 ) ) ;
#15043 = ORIENTED_EDGE ( 'NONE', *, *, #8630, .T. ) ;
#15044 = ORIENTED_EDGE ( 'NONE', *, *, #2364, .F. ) ;
#15045 = ORIENTED_EDGE ( 'NONE', *, *, #12699, .F. ) ;
#15046 = CIRCLE ( 'NONE', #13464, 3.499999999999999556 ) ;
#15047 = CARTESIAN_POINT ( 'NONE',  ( 4.276409079477644148, 1.261996585732577891, -8.312499998634407916 ) ) ;
#15048 = ORIENTED_EDGE ( 'NONE', *, *, #1877, .F. ) ;
#15049 = DIRECTION ( 'NONE',  ( -1.000000000000000000, 0.000000000000000000, 0.000000000000000000 ) ) ;
#15050 = EDGE_CURVE ( 'NONE', #15563, #15506, #14462, .T. ) ;
#15051 = DIRECTION ( 'NONE',  ( 0.000000000000000000, 0.000000000000000000, 1.000000000000000000 ) ) ;
#15052 = CARTESIAN_POINT ( 'NONE',  ( -4.458734125000001214, -30.12500000136559208, 1.846868145590734089 ) ) ;
#15053 = CIRCLE ( 'NONE', #3675, 32.00000000000000711 ) ;
#15054 = AXIS2_PLACEMENT_3D ( 'NONE', #5003, #9930, #14869 ) ;
#15055 = CARTESIAN_POINT ( 'NONE',  ( -2.131511515620587272, -3.916244202832140253, -5.937499998634407028 ) ) ;
#15056 = CARTESIAN_POINT ( 'NONE',  ( -21.01110699893060030, -1.230770033143087371E-15, 39.04230484541322710 ) ) ;
#15057 = ORIENTED_EDGE ( 'NONE', *, *, #9216, .F. ) ;
#15058 = CYLINDRICAL_SURFACE ( 'NONE', #8477, 5.000000000000000888 ) ;
#15059 = ORIENTED_EDGE ( 'NONE', *, *, #12437, .F. ) ;
#15060 = CARTESIAN_POINT ( 'NONE',  ( 1.415196051561583790, -4.795541693661363958, -7.250000000000002665 ) ) ;
#15061 = CARTESIAN_POINT ( 'NONE',  ( 67.49999999999931788, 37.00000000000000000, -2.649999999999971934 ) ) ;
#15062 = ORIENTED_EDGE ( 'NONE', *, *, #9686, .T. ) ;
#15063 = CARTESIAN_POINT ( 'NONE',  ( 3.753672977998667726, 3.033343224707664820, -5.499999998634407916 ) ) ;
#15064 = DIRECTION ( 'NONE',  ( 0.000000000000000000, 1.000000000000000000, 0.000000000000000000 ) ) ;
#15065 = CARTESIAN_POINT ( 'NONE',  ( 5.000000000000000000, -21.18750000273119127, 2.071067811865478614 ) ) ;
#15066 = CARTESIAN_POINT ( 'NONE',  ( -2.071067811865477726, -30.81250000273118062, -4.999999999999996447 ) ) ;
#15067 = CARTESIAN_POINT ( 'NONE',  ( 4.209348295687701302, 3.401574460001765665, -5.812499997268813168 ) ) ;
#15068 = CARTESIAN_POINT ( 'NONE',  ( 1.999999999999998224, -3.464101615137772594, -3.142992957459239012 ) ) ;
#15069 = DIRECTION ( 'NONE',  ( 1.000000000000000000, 0.000000000000000000, -0.000000000000000000 ) ) ;
#15070 = CARTESIAN_POINT ( 'NONE',  ( -4.458734125000000326, -23.12500000136559564, 1.846868145590734089 ) ) ;
#15071 = VERTEX_POINT ( 'NONE', #14536 ) ;
#15072 = CARTESIAN_POINT ( 'NONE',  ( 0.000000000000000000, -11.00000000000000178, 0.000000000000000000 ) ) ;
#15073 = CARTESIAN_POINT ( 'NONE',  ( -3.916244202832140253, 2.131511515620587272, -7.937499998634408804 ) ) ;
#15074 = CARTESIAN_POINT ( 'NONE',  ( 16.55500000000001393, 3.061616997868383634E-16, -2.500000000000000444 ) ) ;
#15075 = EDGE_CURVE ( 'NONE', #12769, #13829, #14615, .T. ) ;
#15076 = ORIENTED_EDGE ( 'NONE', *, *, #15956, .T. ) ;
#15077 = VERTEX_POINT ( 'NONE', #8411 ) ;
#15078 = EDGE_CURVE ( 'NONE', #7896, #6730, #9946, .T. ) ;
#15079 = ORIENTED_EDGE ( 'NONE', *, *, #11261, .F. ) ;
#15080 = CARTESIAN_POINT ( 'NONE',  ( 0.000000000000000000, 37.00000000000000000, 0.000000000000000000 ) ) ;
#15081 = DIRECTION ( 'NONE',  ( -0.000000000000000000, 1.000000000000000000, -0.000000000000000000 ) ) ;
#15082 = CARTESIAN_POINT ( 'NONE',  ( 7.102951435054648059E-15, 40.00000000000000000, 57.99999999999999289 ) ) ;
#15083 = B_SPLINE_CURVE_WITH_KNOTS ( 'NONE', 3,
 ( #3602, #11116, #3843, #11274, #10075, #3916 ),
 .UNSPECIFIED., .F., .F.,
 ( 4, 2, 4 ),
 ( -3.640115492410698714E-06, 0.0002066546034006521879, 0.0004169493222937151081 ),
 .UNSPECIFIED. ) ;
#15084 =( GEOMETRIC_REPRESENTATION_CONTEXT ( 3 ) GLOBAL_UNCERTAINTY_ASSIGNED_CONTEXT ( ( #8691 ) ) GLOBAL_UNIT_ASSIGNED_CONTEXT ( ( #11921, #3294, #8245 ) ) REPRESENTATION_CONTEXT ( 'NONE', 'WORKASPACE' ) );
#15085 = DIRECTION ( 'NONE',  ( 1.000000000000000000, 0.000000000000000000, 0.000000000000000000 ) ) ;
#15086 = DIRECTION ( 'NONE',  ( 1.000000000000000000, 0.000000000000000000, 0.000000000000000000 ) ) ;
#15087 = CARTESIAN_POINT ( 'NONE',  ( 4.000000000000000000, -2.309401076758514915, -5.000000000000000000 ) ) ;
#15088 = CARTESIAN_POINT ( 'NONE',  ( -0.5711823568785978633, -5.381735091635035495, -6.312500000000000888 ) ) ;
#15089 = CARTESIAN_POINT ( 'NONE',  ( -28.86751345947056180, -5.000000000000000000, -20.00000000000000355 ) ) ;
#15090 = CARTESIAN_POINT ( 'NONE',  ( -3.152801135295367096, -22.06250000136559564, -3.152801135295367541 ) ) ;
#15091 = CARTESIAN_POINT ( 'NONE',  ( -3.753672977998669946, -3.033343224707661712, -6.999999998634408804 ) ) ;
#15092 = VERTEX_POINT ( 'NONE', #15601 ) ;
#15093 = EDGE_CURVE ( 'NONE', #8967, #6357, #2976, .T. ) ;
#15094 = EDGE_LOOP ( 'NONE', ( #5817, #13809, #3957, #718 ) ) ;
#15095 = ORIENTED_EDGE ( 'NONE', *, *, #13110, .F. ) ;
#15096 = EDGE_CURVE ( 'NONE', #9678, #1654, #674, .T. ) ;
#15097 = PRODUCT_RELATED_PRODUCT_CATEGORY ( 'part', '', ( #3575 ) ) ;
#15098 = AXIS2_PLACEMENT_3D ( 'NONE', #8940, #2782, #7740 ) ;
#15099 = CARTESIAN_POINT ( 'NONE',  ( -3.152801135295367096, -22.06250000136559564, -3.152801135295367541 ) ) ;
#15100 = DIRECTION ( 'NONE',  ( 1.000000000000000000, -1.387778780781446464E-15, 0.000000000000000000 ) ) ;
#15101 = AXIS2_PLACEMENT_3D ( 'NONE', #12299, #13502, #14434 ) ;
#15102 = EDGE_LOOP ( 'NONE', ( #2290, #1252 ) ) ;
#15103 = CARTESIAN_POINT ( 'NONE',  ( 4.175648173966055587, -2.207990556236547608, -3.469390959564065291 ) ) ;
#15104 = FACE_OUTER_BOUND ( 'NONE', #15944, .T. ) ;
#15105 = CARTESIAN_POINT ( 'NONE',  ( -44.99999999999999289, -13.00000000000000178, 4.000000000000831335 ) ) ;
#15106 = DIRECTION ( 'NONE',  ( -0.000000000000000000, -1.000000000000000000, -0.000000000000000000 ) ) ;
#15107 = CARTESIAN_POINT ( 'NONE',  ( -2.071067811865478170, -31.31250000000000000, 5.000000000000000000 ) ) ;
#15108 =( GEOMETRIC_REPRESENTATION_CONTEXT ( 3 ) GLOBAL_UNCERTAINTY_ASSIGNED_CONTEXT ( ( #13052 ) ) GLOBAL_UNIT_ASSIGNED_CONTEXT ( ( #5255, #3801, #8903 ) ) REPRESENTATION_CONTEXT ( 'NONE', 'WORKASPACE' ) );
#15109 = CARTESIAN_POINT ( 'NONE',  ( -3.511755186886750479, 2.826662030176366081, -3.597382984111578086 ) ) ;
#15110 = LINE ( 'NONE', #14963, #8474 ) ;
#15111 = CARTESIAN_POINT ( 'NONE',  ( 3.061616997868383141E-16, -23.87500000273118772, -5.000000000000000000 ) ) ;
#15112 = CYLINDRICAL_SURFACE ( 'NONE', #5227, 2.000000000000000888 ) ;
#15113 = CARTESIAN_POINT ( 'NONE',  ( 3.152801135295367541, -26.31250000136559564, -3.152801135295367541 ) ) ;
#15114 = EDGE_CURVE ( 'NONE', #1389, #5622, #9687, .T. ) ;
#15115 = ORIENTED_EDGE ( 'NONE', *, *, #12797, .T. ) ;
#15116 = EDGE_LOOP ( 'NONE', ( #3621, #8420, #3338, #5116, #13227 ) ) ;
#15117 = ADVANCED_FACE ( 'NONE', ( #12576 ), #2559, .T. ) ;
#15118 = APPLICATION_PROTOCOL_DEFINITION ( 'draft international standard', 'automotive_design', 1998, #8986 ) ;
#15119 = ORIENTED_EDGE ( 'NONE', *, *, #2112, .T. ) ;
#15120 = CARTESIAN_POINT ( 'NONE',  ( 3.678949249685231848, 0.000000000000000000, 0.000000000000000000 ) ) ;
#15121 = AXIS2_PLACEMENT_3D ( 'NONE', #9379, #10894, #10746 ) ;
#15122 = ORIENTED_EDGE ( 'NONE', *, *, #4312, .T. ) ;
#15123 = CARTESIAN_POINT ( 'NONE',  ( 16.55500000000001393, 0.000000000000000000, 0.000000000000000000 ) ) ;
#15124 = AXIS2_PLACEMENT_3D ( 'NONE', #8270, #10435, #9540 ) ;
#15125 = CIRCLE ( 'NONE', #6834, 2.700000000000001066 ) ;
#15126 = CARTESIAN_POINT ( 'NONE',  ( -21.01110699893041911, -3.000000000000001332, -36.39230484541334221 ) ) ;
#15127 = CARTESIAN_POINT ( 'NONE',  ( 4.795541693661363958, 1.415196051561583790, -6.874999997268815832 ) ) ;
#15128 = ITEM_DEFINED_TRANSFORMATION ( 'NONE', 'NONE', #1659,  #3223 ) ;
#15129 =( BOUNDED_CURVE ( )  B_SPLINE_CURVE ( 2, ( #4231, #5529, #10463, #4321, #9260, #8049, #14184, #12947, #5614, #5762, #14335 ),
 .UNSPECIFIED., .F., .F. ) 
 B_SPLINE_CURVE_WITH_KNOTS ( ( 3, 2, 2, 2, 2, 3 ),
 ( 0.3545872658012772516, 0.3624999999999999889, 0.3750000000000000000, 0.3875000000000000111, 0.4000000000000000222, 0.4045872658012772960 ),
 .UNSPECIFIED. ) 
 CURVE ( )  GEOMETRIC_REPRESENTATION_ITEM ( )  RATIONAL_B_SPLINE_CURVE ( ( 0.9646335149384808183, 0.9518143178943437865, 1.000000000000000000, 0.9238795325112867385, 1.000000000000000000, 0.9238795325112867385, 1.000000000000000000, 0.9238795325112867385, 1.000000000000000000, 0.9720652146169428409, 0.9646335149384805963 ) ) 
 REPRESENTATION_ITEM ( '' )  );
#15130 = SHAPE_REPRESENTATION ( 'connector', ( #3223 ), #1938 ) ;
#15131 = VECTOR ( 'NONE', #222, 1000.000000000000000 ) ;
#15132 = CARTESIAN_POINT ( 'NONE',  ( 4.276409079477644148, 1.261996585732577891, -3.562499998634407916 ) ) ;
#15133 = DIRECTION ( 'NONE',  ( 0.000000000000000000, 0.000000000000000000, 1.000000000000000000 ) ) ;
#15134 = VERTEX_POINT ( 'NONE', #4837 ) ;
#15135 = VECTOR ( 'NONE', #10655, 1000.000000000000000 ) ;
#15136 = CARTESIAN_POINT ( 'NONE',  ( 4.107478936458598184, -3.387975324182885828, -48.68990028668294912 ) ) ;
#15137 = EDGE_CURVE ( 'NONE', #8451, #6399, #6378, .T. ) ;
#15138 =( NAMED_UNIT ( * ) SI_UNIT ( $, .STERADIAN. ) SOLID_ANGLE_UNIT ( ) );
#15139 = ORIENTED_EDGE ( 'NONE', *, *, #520, .T. ) ;
#15140 = CARTESIAN_POINT ( 'NONE',  ( -4.795541693661363958, -1.415196051561583790, -7.500000000000003553 ) ) ;
#15141 = DIRECTION ( 'NONE',  ( 1.000000000000000000, 0.000000000000000000, 0.000000000000000000 ) ) ;
#15142 = EDGE_LOOP ( 'NONE', ( #12899, #12373, #7859, #15043 ) ) ;
#15143 = CARTESIAN_POINT ( 'NONE',  ( 4.799145180956616130, -0.5093500532425063732, -7.624999998634407916 ) ) ;
#15144 = CIRCLE ( 'NONE', #939, 4.250000000000000000 ) ;
#15145 = CARTESIAN_POINT ( 'NONE',  ( 5.000000000000000888, 0.000000000000000000, -25.03750572909317285 ) ) ;
#15146 = PRODUCT_DEFINITION_SHAPE ( 'NONE', 'NONE',  #15992 ) ;
#15147 = CARTESIAN_POINT ( 'NONE',  ( -4.276409079477644148, -1.261996585732578335, -7.812499998634407916 ) ) ;
#15148 = VECTOR ( 'NONE', #8755, 1000.000000000000000 ) ;
#15149 = PLANE ( 'NONE',  #5135 ) ;
#15150 = VECTOR ( 'NONE', #1655, 1000.000000000000000 ) ;
#15151 = DIRECTION ( 'NONE',  ( -1.000000000000000000, 0.000000000000000000, -0.000000000000000000 ) ) ;
#15152 = CARTESIAN_POINT ( 'NONE',  ( -2.390265326283148806, -4.391654775818394363, -3.249999997268816276 ) ) ;
#15153 = DIRECTION ( 'NONE',  ( -1.000000000000000000, 0.000000000000000000, 0.000000000000000000 ) ) ;
#15154 = VECTOR ( 'NONE', #8614, 1000.000000000000000 ) ;
#15155 = CARTESIAN_POINT ( 'NONE',  ( 0.000000000000000000, 0.000000000000000000, -0.3080913168122742518 ) ) ;
#15156 = CARTESIAN_POINT ( 'NONE',  ( 6.123233995736766282E-16, -20.00000000000000000, -5.000000000000000000 ) ) ;
#15157 = ORIENTED_EDGE ( 'NONE', *, *, #14558, .F. ) ;
#15158 = DIRECTION ( 'NONE',  ( 0.000000000000000000, 0.000000000000000000, -1.000000000000000000 ) ) ;
#15159 = CARTESIAN_POINT ( 'NONE',  ( 4.799145180956616130, -0.5093500532425063732, -6.374999998634407028 ) ) ;
#15160 = ADVANCED_FACE ( 'NONE', ( #73 ), #4991, .F. ) ;
#15161 = CARTESIAN_POINT ( 'NONE',  ( 0.000000000000000000, -20.00000000000000000, 5.000000000000000000 ) ) ;
#15162 = VERTEX_POINT ( 'NONE', #2640 ) ;
#15163 = EDGE_LOOP ( 'NONE', ( #7766, #10563 ) ) ;
#15164 = AXIS2_PLACEMENT_3D ( 'NONE', #7632, #33, #8598 ) ;
#15165 = VERTEX_POINT ( 'NONE', #10007 ) ;
#15166 = CARTESIAN_POINT ( 'NONE',  ( 10.17949192431120586, 0.000000000000000000, 57.63139720814412925 ) ) ;
#15167 = DIRECTION ( 'NONE',  ( 0.000000000000000000, 0.000000000000000000, 1.000000000000000000 ) ) ;
#15168 = DIRECTION ( 'NONE',  ( -0.4999999999999997780, 0.000000000000000000, -0.8660254037844388186 ) ) ;
#15169 = VECTOR ( 'NONE', #11030, 1000.000000000000000 ) ;
#15170 = EDGE_CURVE ( 'NONE', #3351, #1389, #8542, .T. ) ;
#15171 = LINE ( 'NONE', #4982, #10762 ) ;
#15172 = DIRECTION ( 'NONE',  ( -0.000000000000000000, -1.000000000000000000, -0.000000000000000000 ) ) ;
#15173 = LINE ( 'NONE', #1587, #2033 ) ;
#15174 = VECTOR ( 'NONE', #9336, 1000.000000000000000 ) ;
#15175 = AXIS2_PLACEMENT_3D ( 'NONE', #7897, #5151, #10080 ) ;
#15176 = CARTESIAN_POINT ( 'NONE',  ( 2.390265326283148806, 4.391654775818395251, -6.875000000000002665 ) ) ;
#15177 = CARTESIAN_POINT ( 'NONE',  ( 4.209348295687701302, 3.401574460001766109, -2.937500000000003553 ) ) ;
#15178 = CARTESIAN_POINT ( 'NONE',  ( -3.453038570459499024, -2.625189405340453419, -3.535263753545272891 ) ) ;
#15179 = CARTESIAN_POINT ( 'NONE',  ( -1.846868145590734756, -22.12500000136559564, -4.458734125000000326 ) ) ;
#15180 = CARTESIAN_POINT ( 'NONE',  ( 3.753672977998667726, 3.033343224707664376, -8.499999998634411469 ) ) ;
#15181 = ORIENTED_EDGE ( 'NONE', *, *, #86, .T. ) ;
#15182 = AXIS2_PLACEMENT_3D ( 'NONE', #1987, #14279, #4495 ) ;
#15183 = CARTESIAN_POINT ( 'NONE',  ( -4.000000000000000000, -2.309401076758512694, -3.433295621305382461 ) ) ;
#15184 = ORIENTED_EDGE ( 'NONE', *, *, #11532, .F. ) ;
#15185 = ORIENTED_EDGE ( 'NONE', *, *, #3213, .T. ) ;
#15186 = EDGE_LOOP ( 'NONE', ( #10260, #344, #5579, #7577, #3417, #4206 ) ) ;
#15187 = APPLICATION_CONTEXT ( 'automotive_design' ) ;
#15188 = CARTESIAN_POINT ( 'NONE',  ( 4.458734124999999437, -31.68750000136559564, 0.000000000000000000 ) ) ;
#15189 = CARTESIAN_POINT ( 'NONE',  ( 47.32050807568875683, -37.00000000000000711, 41.96152422706633445 ) ) ;
#15190 = ORIENTED_EDGE ( 'NONE', *, *, #11836, .T. ) ;
#15191 = AXIS2_PLACEMENT_3D ( 'NONE', #5982, #10905, #2484 ) ;
#15192 = FACE_OUTER_BOUND ( 'NONE', #13246, .T. ) ;
#15193 = DIRECTION ( 'NONE',  ( 0.000000000000000000, 0.000000000000000000, 1.000000000000000000 ) ) ;
#15194 = EDGE_CURVE ( 'NONE', #11803, #7219, #1001, .T. ) ;
#15195 = CARTESIAN_POINT ( 'NONE',  ( -0.5093500532425060401, -4.799145180956616130, -0.6249999986344054737 ) ) ;
#15196 = CARTESIAN_POINT ( 'NONE',  ( -7.500000000000001776, 0.000000000000000000, 0.000000000000000000 ) ) ;
#15197 = EDGE_CURVE ( 'NONE', #8765, #12673, #12490, .T. ) ;
#15198 = AXIS2_PLACEMENT_3D ( 'NONE', #2336, #15928, #2254 ) ;
#15199 = CARTESIAN_POINT ( 'NONE',  ( -3.535533905932737309, -31.62500000000000000, -3.535533905932738197 ) ) ;
#15200 = CARTESIAN_POINT ( 'NONE',  ( -2.131511515620587272, -3.916244202832140253, -4.687499998634405252 ) ) ;
#15201 = CARTESIAN_POINT ( 'NONE',  ( 3.061616997868383141E-16, -21.87500000273118772, -5.000000000000000000 ) ) ;
#15202 = CIRCLE ( 'NONE', #7985, 5.000000000000000000 ) ;
#15203 = CARTESIAN_POINT ( 'NONE',  ( -24.26932219902319687, 40.00000000000000000, 5.999999999999998224 ) ) ;
#15204 = CARTESIAN_POINT ( 'NONE',  ( 2.071067811865475505, -22.93750000273119127, -5.000000000000000888 ) ) ;
#15205 = DIRECTION ( 'NONE',  ( 0.000000000000000000, -0.000000000000000000, 1.000000000000000000 ) ) ;
#15206 = AXIS2_PLACEMENT_3D ( 'NONE', #6327, #11402, #10205 ) ;
#15207 = CARTESIAN_POINT ( 'NONE',  ( 1.846868145590736310, -27.62500000136559564, 4.458734124999997661 ) ) ;
#15208 = FACE_OUTER_BOUND ( 'NONE', #4392, .T. ) ;
#15209 = ORIENTED_EDGE ( 'NONE', *, *, #9108, .F. ) ;
#15210 = ORIENTED_EDGE ( 'NONE', *, *, #7624, .F. ) ;
#15211 = VERTEX_POINT ( 'NONE', #11134 ) ;
#15212 = CARTESIAN_POINT ( 'NONE',  ( 4.211140560182196957, -2.431303136016555122, -3.745885042887436622 ) ) ;
#15213 = VECTOR ( 'NONE', #14669, 1000.000000000000000 ) ;
#15214 = CIRCLE ( 'NONE', #12349, 2.649999999999985700 ) ;
#15215 = ORIENTED_EDGE ( 'NONE', *, *, #14329, .T. ) ;
#15216 = LINE ( 'NONE', #2668, #2234 ) ;
#15217 = EDGE_CURVE ( 'NONE', #14724, #307, #8931, .T. ) ;
#15218 = B_SPLINE_CURVE_WITH_KNOTS ( 'NONE', 3,
 ( #4794, #13581, #5271, #2511, #11170, #2763, #1558, #1474, #10212, #15136, #4056, #12374, #7634, #3819, #11253, #9006 ),
 .UNSPECIFIED., .F., .F.,
 ( 4, 2, 2, 2, 2, 2, 2, 4 ),
 ( 1.833078488450472941E-15, 0.0003988053453855977407, 0.0007976106907693624208, 0.001196416036153127209, 0.001595221381536891889, 0.002392832072304423418, 0.002791637417688189182, 0.003190442763071954946 ),
 .UNSPECIFIED. ) ;
#15219 = DIRECTION ( 'NONE',  ( 0.000000000000000000, 0.000000000000000000, 1.000000000000000000 ) ) ;
#15220 = EDGE_CURVE ( 'NONE', #14249, #8490, #13707, .T. ) ;
#15221 = CARTESIAN_POINT ( 'NONE',  ( -2.390265326283148806, -4.391654775818394363, -4.249999997268816720 ) ) ;
#15222 = DIRECTION ( 'NONE',  ( 0.000000000000000000, 0.000000000000000000, -1.000000000000000000 ) ) ;
#15223 = CARTESIAN_POINT ( 'NONE',  ( 2.390265326283148806, 4.391654775818395251, -7.749999997268816720 ) ) ;
#15224 = AXIS2_PLACEMENT_3D ( 'NONE', #4541, #3250, #8199 ) ;
#15225 = DIRECTION ( 'NONE',  ( -1.000000000000000000, 0.000000000000000000, 0.000000000000000000 ) ) ;
#15226 = ORIENTED_EDGE ( 'NONE', *, *, #7377, .T. ) ;
#15227 = EDGE_LOOP ( 'NONE', ( #1433, #3493, #5196, #14463 ) ) ;
#15228 = CARTESIAN_POINT ( 'NONE',  ( -21.01110699893060030, 2.000000000000000000, 33.74230484541324415 ) ) ;
#15229 = LINE ( 'NONE', #6422, #3280 ) ;
#15230 = VERTEX_POINT ( 'NONE', #13630 ) ;
#15231 = CARTESIAN_POINT ( 'NONE',  ( -3.753672977998669502, -3.033343224707661712, -7.999999998634411469 ) ) ;
#15232 = EDGE_CURVE ( 'NONE', #11992, #5212, #8666, .T. ) ;
#15233 = DIRECTION ( 'NONE',  ( 0.000000000000000000, 0.000000000000000000, 1.000000000000000000 ) ) ;
#15234 = EDGE_CURVE ( 'NONE', #2790, #14420, #7123, .T. ) ;
#15235 = ADVANCED_FACE ( 'NONE', ( #10094 ), #12008, .T. ) ;
#15236 =( BOUNDED_CURVE ( )  B_SPLINE_CURVE ( 2, ( #8129, #5763, #10916, #14720, #3557, #6912, #9787, #13026, #614 ),
 .UNSPECIFIED., .F., .F. ) 
 B_SPLINE_CURVE_WITH_KNOTS ( ( 3, 2, 2, 2, 3 ),
 ( 0.6749999999999999334, 0.6874999999999998890, 0.6999999999999999556, 0.7125000000000000222, 0.7249999999999999778 ),
 .UNSPECIFIED. ) 
 CURVE ( )  GEOMETRIC_REPRESENTATION_ITEM ( )  RATIONAL_B_SPLINE_CURVE ( ( 1.000000000000000666, 0.9238795325112860723, 1.000000000000000000, 0.9238795325112867385, 1.000000000000000000, 0.9238795325112867385, 1.000000000000000000, 0.9238795325112867385, 1.000000000000000000 ) ) 
 REPRESENTATION_ITEM ( '' )  );
#15237 = ADVANCED_FACE ( 'NONE', ( #13454 ), #3761, .T. ) ;
#15238 = CARTESIAN_POINT ( 'NONE',  ( -3.535533905932738641, -28.50000000273118772, 3.535533905932737309 ) ) ;
#15239 = CARTESIAN_POINT ( 'NONE',  ( -2.390265326283148806, -4.391654775818394363, -8.249999997268814056 ) ) ;
#15240 = CARTESIAN_POINT ( 'NONE',  ( -2.390265326283148806, -4.391654775818394363, -6.249999997268814944 ) ) ;
#15241 = CARTESIAN_POINT ( 'NONE',  ( 4.795541693661363958, 1.415196051561583790, -8.874999997268814056 ) ) ;
#15242 = DIRECTION ( 'NONE',  ( 0.000000000000000000, 0.000000000000000000, -1.000000000000000000 ) ) ;
#15243 = CARTESIAN_POINT ( 'NONE',  ( 3.152801135295366208, -22.81250000136559564, 3.152801135295367985 ) ) ;
#15244 = ORIENTED_EDGE ( 'NONE', *, *, #11316, .T. ) ;
#15245 = PLANE ( 'NONE',  #7440 ) ;
#15246 = CARTESIAN_POINT ( 'NONE',  ( -4.276409079477644148, -1.261996585732578335, -6.812499998634407028 ) ) ;
#15247 = PLANE ( 'NONE',  #4263 ) ;
#15248 = ORIENTED_EDGE ( 'NONE', *, *, #10175, .T. ) ;
#15249 = CARTESIAN_POINT ( 'NONE',  ( -4.000000000000000000, 1.677772373332757194, -3.535253723897187506 ) ) ;
#15250 = ORIENTED_EDGE ( 'NONE', *, *, #2887, .T. ) ;
#15251 = ORIENTED_EDGE ( 'NONE', *, *, #7629, .T. ) ;
#15252 = CARTESIAN_POINT ( 'NONE',  ( -0.6511518506208979762, 8.763486134561274454, -7.907570769506046204 ) ) ;
#15253 = CYLINDRICAL_SURFACE ( 'NONE', #187, 2.649999999999992806 ) ;
#15254 = CARTESIAN_POINT ( 'NONE',  ( 0.000000000000000000, -20.00000000000000000, 0.000000000000000000 ) ) ;
#15255 = EDGE_CURVE ( 'NONE', #1967, #6711, #1349, .T. ) ;
#15256 = CARTESIAN_POINT ( 'NONE',  ( -35.00000000000000000, 50.00000000000000000, 0.000000000000000000 ) ) ;
#15257 = CARTESIAN_POINT ( 'NONE',  ( -7.777900015783941967, -4.169681370001539378, -7.928862157988302073 ) ) ;
#15258 = PLANE ( 'NONE',  #12855 ) ;
#15259 = CARTESIAN_POINT ( 'NONE',  ( 4.795541693661363958, 1.415196051561583790, -6.000000000000001776 ) ) ;
#15260 = CARTESIAN_POINT ( 'NONE',  ( -35.00000000000000000, 40.00000000000000000, -5.999999999999991118 ) ) ;
#15261 = FACE_OUTER_BOUND ( 'NONE', #4200, .T. ) ;
#15262 = CARTESIAN_POINT ( 'NONE',  ( -44.99999999999999289, -35.00000000000000000, -7.500000000000000000 ) ) ;
#15263 = CARTESIAN_POINT ( 'NONE',  ( -4.276409079477644148, -1.261996585732578335, -6.062499998634407028 ) ) ;
#15264 = ORIENTED_EDGE ( 'NONE', *, *, #908, .T. ) ;
#15265 = CARTESIAN_POINT ( 'NONE',  ( 7.808623696107861889, -4.508310992946700679, -7.999704684617483963 ) ) ;
#15266 = VERTEX_POINT ( 'NONE', #2720 ) ;
#15267 = VERTEX_POINT ( 'NONE', #2395 ) ;
#15268 = EDGE_LOOP ( 'NONE', ( #15724, #8195, #2835, #14263 ) ) ;
#15269 = CARTESIAN_POINT ( 'NONE',  ( -1.846868145590737420, -21.75000000136559564, 4.458734124999999437 ) ) ;
#15270 = EDGE_CURVE ( 'NONE', #11871, #15747, #11063, .T. ) ;
#15271 = CARTESIAN_POINT ( 'NONE',  ( -1.415196051561583790, 4.795541693661363958, -7.750000000000003553 ) ) ;
#15272 = VERTEX_POINT ( 'NONE', #10408 ) ;
#15273 = CARTESIAN_POINT ( 'NONE',  ( -44.99999999999999289, -13.00000000000000178, -3.999999999999170885 ) ) ;
#15274 = CARTESIAN_POINT ( 'NONE',  ( -28.86751345948129455, -37.00000000000000711, 20.00000000000000355 ) ) ;
#15275 = CARTESIAN_POINT ( 'NONE',  ( -3.033343224707664820, 3.753672977998667726, -1.999999998634408360 ) ) ;
#15276 = CARTESIAN_POINT ( 'NONE',  ( 3.962264623424024190, 2.061996207999744701, -0.3789984458506767684 ) ) ;
#15277 = CARTESIAN_POINT ( 'NONE',  ( 5.000000000000000888, -26.93750000000000711, -2.071067811865475505 ) ) ;
#15278 = CARTESIAN_POINT ( 'NONE',  ( 3.916244202832140253, -2.131511515620588160, -3.437499998634407916 ) ) ;
#15279 = CARTESIAN_POINT ( 'NONE',  ( -44.43375672972887003, -4.730053418719387004, -19.99999999999998934 ) ) ;
#15280 = DIRECTION ( 'NONE',  ( -1.000000000000000000, -0.000000000000000000, -0.000000000000000000 ) ) ;
#15281 = CARTESIAN_POINT ( 'NONE',  ( 2.071067811865476394, -23.31250000273118772, 5.000000000000000000 ) ) ;
#15282 = DIRECTION ( 'NONE',  ( 0.000000000000000000, 0.000000000000000000, -1.000000000000000000 ) ) ;
#15283 = CARTESIAN_POINT ( 'NONE',  ( -4.458734124999999437, -24.93750000136559564, -5.460374474430324690E-16 ) ) ;
#15284 = CARTESIAN_POINT ( 'NONE',  ( 7.169303301815073581, -4.521054846639389169, -7.349897473155027505 ) ) ;
#15285 = ORIENTED_EDGE ( 'NONE', *, *, #8608, .F. ) ;
#15286 = VERTEX_POINT ( 'NONE', #2809 ) ;
#15287 = CARTESIAN_POINT ( 'NONE',  ( 0.000000000000000000, 0.000000000000000000, -60.00000000000000000 ) ) ;
#15288 = PRODUCT_DEFINITION_SHAPE ( 'NONE', 'NONE',  #15985 ) ;
#15290 = ORIENTED_EDGE ( 'NONE', *, *, #10222, .F. ) ;
#15289 = EDGE_CURVE ( 'NONE', #9472, #10300, #4023, .T. ) ;
#15291 = CARTESIAN_POINT ( 'NONE',  ( -8.673617379884035472E-16, -9.147862274876560562, -8.047472243342939535 ) ) ;
#15292 = AXIS2_PLACEMENT_3D ( 'NONE', #3396, #4454, #6891 ) ;
#15293 = ADVANCED_FACE ( 'NONE', ( #4260 ), #10494, .T. ) ;
#15294 = VERTEX_POINT ( 'NONE', #1909 ) ;
#15295 = FACE_OUTER_BOUND ( 'NONE', #13285, .T. ) ;
#15296 = PLANE ( 'NONE',  #8101 ) ;
#15297 = CARTESIAN_POINT ( 'NONE',  ( 3.152801135295366208, -30.81250000136559564, 3.152801135295367985 ) ) ;
#15298 = CARTESIAN_POINT ( 'NONE',  ( 2.500000000000000000, -2.357898499370432610, 3.252606517456513302E-15 ) ) ;
#15299 = CARTESIAN_POINT ( 'NONE',  ( 2.131511515620586383, 3.916244202832140253, -8.437499998634409692 ) ) ;
#15300 = CARTESIAN_POINT ( 'NONE',  ( 4.799145180956616130, -0.5093500532425063732, 1.375000001365592528 ) ) ;
#15301 = ORIENTED_EDGE ( 'NONE', *, *, #15734, .T. ) ;
#15302 = APPLICATION_PROTOCOL_DEFINITION ( 'draft international standard', 'automotive_design', 1998, #4842 ) ;
#15303 = EDGE_LOOP ( 'NONE', ( #1504, #11609, #15454, #272 ) ) ;
#15304 = CARTESIAN_POINT ( 'NONE',  ( 2.500000000000000000, -2.357898499370432610, 3.252606517456513302E-15 ) ) ;
#15305 = CARTESIAN_POINT ( 'NONE',  ( 2.730187237215162345E-16, -27.18750000136559564, -4.458734124999999437 ) ) ;
#15306 = EDGE_CURVE ( 'NONE', #11064, #3993, #933, .T. ) ;
#15307 = ORIENTED_EDGE ( 'NONE', *, *, #10670, .F. ) ;
#15308 = VECTOR ( 'NONE', #10119, 1000.000000000000000 ) ;
#15309 = DIRECTION ( 'NONE',  ( -0.8191520442889907994, 1.003171929053523514E-16, 0.5735764363510474917 ) ) ;
#15310 = AXIS2_PLACEMENT_3D ( 'NONE', #9732, #3428, #9574 ) ;
#15311 = CARTESIAN_POINT ( 'NONE',  ( -115.0000000000000142, -10.00000000000000888, 7.500000000000001776 ) ) ;
#15312 = CARTESIAN_POINT ( 'NONE',  ( 1.317756351988342622, -3.857995168970215438, -0.04852650426602527628 ) ) ;
#15313 = VECTOR ( 'NONE', #7426, 999.9999999999998863 ) ;
#15314 = PRODUCT_DEFINITION_CONTEXT ( 'detailed design', #99, 'design' ) ;
#15315 = CARTESIAN_POINT ( 'NONE',  ( 4.391654775818395251, -2.390265326283149694, -6.999999997268815832 ) ) ;
#15316 = CARTESIAN_POINT ( 'NONE',  ( 0.5711823568785988625, 5.381735091635026613, -0.8124999999999997780 ) ) ;
#15317 = CARTESIAN_POINT ( 'NONE',  ( 42.02221399786069611, 2.000000000000000000, 2.650000000000100275 ) ) ;
#15318 = CARTESIAN_POINT ( 'NONE',  ( 4.458734124999999437, -23.68750000136559564, 0.000000000000000000 ) ) ;
#15319 = ORIENTED_EDGE ( 'NONE', *, *, #3088, .T. ) ;
#15320 = CARTESIAN_POINT ( 'NONE',  ( -81.33974596215558961, -105.7735026918962404, 7.500000000000001776 ) ) ;
#15321 = CARTESIAN_POINT ( 'NONE',  ( 7.500000000000003553, -4.330127018922199866, -7.422398894150035176 ) ) ;
#15322 = CIRCLE ( 'NONE', #4981, 2.500000000000000444 ) ;
#15323 = CARTESIAN_POINT ( 'NONE',  ( 0.000000000000000000, 0.000000000000000000, 0.000000000000000000 ) ) ;
#15324 = EDGE_CURVE ( 'NONE', #4537, #10561, #12898, .T. ) ;
#15325 = ORIENTED_EDGE ( 'NONE', *, *, #9216, .T. ) ;
#15326 = CARTESIAN_POINT ( 'NONE',  ( 2.500000000000000000, -1.178949249685213863, 2.042000000000002924 ) ) ;
#15327 = ORIENTED_EDGE ( 'NONE', *, *, #12520, .F. ) ;
#15328 = EDGE_CURVE ( 'NONE', #15838, #1307, #7912, .T. ) ;
#15329 = ORIENTED_EDGE ( 'NONE', *, *, #15050, .T. ) ;
#15330 = DIRECTION ( 'NONE',  ( 0.000000000000000000, 0.000000000000000000, 1.000000000000000000 ) ) ;
#15331 = CARTESIAN_POINT ( 'NONE',  ( -0.6640947660597427138, 4.471078309994878985, -3.602146406945963442 ) ) ;
#15332 =( BOUNDED_SURFACE ( )  B_SPLINE_SURFACE ( 1, 2, ( 
 ( #2215, #9649, #4964, #48, #8310, #12306, #7402, #13508, #12558, #2373, #11109, #7169, #10948, #4810, #12071, #9734, #1015, #14671, #7085, #1245, #9817, #5948, #9891, #15810, #8544, #2445, #10868, #4727, #7248, #937, #11986, #3670, #13200, #4651, #2138, #3596, #12221, #14584, #9576, #4891, #12148, #1163, #3504, #13432, #14747, #8463, #13362, #2303, #6105, #13848, #8779, #4070, #6267, #2778, #13927, #11499, #1322, #2530, #11181, #7565, #449, #10143, #12387, #5372, #6508, #12548, #369, #12463, #14828, #9024, #15152, #2853, #3747, #126, #7808, #11346, #11422, #7737, #6348, #3908, #8854, #3836, #8693, #5286, #12628, #12703, #3984, #1643, #6584, #5047, #10067, #9976, #1495, #6435, #1569, #13598, #14915, #7484, #13681, #2612, #10226, #1402, #11267, #215, #5136, #14996, #13759, #2693, #298, #7651, #5208, #15067, #8937, #6823, #4228, #610, #11890, #6991, #15240, #3260, #14333, #4472, #1962, #9331, #13107, #5452, #8047, #11730, #10383, #12945, #15315, #5611, #14002, #8207, #766, #9174, #838, #6751, #15481, #9406, #14095, #3019, #14182, #7885, #2930, #10624, #10315, #12781, #4149, #685, #3181, #7966, #535, #6908, #3109, #8126, #10461, #10552, #11816, #9095, #2046 ),
 ( #12869, #1804, #4399, #14255, #11655, #1723, #15555, #6674, #5527, #15395, #11583, #4318, #9258, #1881, #13023, #5687, #6084, #12130, #5845, #7068, #7302, #7148, #11967, #9714, #9485, #5760, #12051, #2117, #3654, #10851, #5930, #14490, #3486, #13181, #15791, #13338, #996, #15634, #15952, #8597, #4709, #9630, #4877, #14564, #10779, #2425, #9802, #919, #8446, #12204, #1144, #2283, #8525, #15720, #3411, #2355, #8363, #4633, #7232, #14730, #13487, #1067, #6003, #10929, #14651, #15868, #7379, #8292, #10697, #9561, #13255, #4790, #3576, #2197, #13418, #11014, #12289, #4552, #14417, #3343, #15132, #11095, #13576, #12526, #355, #13913, #3728, #4948, #8674, #9955, #2840, #1470, #14807, #7792, #8919, #14979, #2760, #14895, #1224, #11405, #1553, #1384, #6174, #6413, #6329, #11331, #106, #5025, #5268, #31, #5111, #2506, #7467, #12371, #6250, #1304, #5193, #11165, #15055, #9876, #3814, #11248, #8762, #13663, #6493, #10208, #9002, #4053, #10048, #195, #2593, #7547, #12447, #3891, #8836, #13739, #13827, #2672, #7630, #280, #10123, #3968, #7715, #12610, #11800, #591, #1710, #9394, #752, #2918, #1793, #14243, #3167, #12853, #15467, #7868, #10370, #9320, #15299, #12765, #7951 ) ),
 .UNSPECIFIED., .F., .F., .F. ) 
 B_SPLINE_SURFACE_WITH_KNOTS ( ( 2, 2 ),
 ( 3, 2, 2, 2, 2, 2, 2, 2, 2, 2, 2, 2, 2, 2, 2, 2, 2, 2, 2, 2, 2, 2, 2, 2, 2, 2, 2, 2, 2, 2, 2, 2, 2, 2, 2, 2, 2, 2, 2, 2, 2, 2, 2, 2, 2, 2, 2, 2, 2, 2, 2, 2, 2, 2, 2, 2, 2, 2, 2, 2, 2, 2, 2, 2, 2, 2, 2, 2, 2, 2, 2, 2, 2, 2, 2, 2, 2, 2, 2, 2, 3 ),
 ( 0.000000000000000000, 1.000000000000000000 ),
 ( 0.000000000000000000, 0.01250000000000000069, 0.02500000000000000139, 0.03749999999999999861, 0.05000000000000000278, 0.06250000000000000000, 0.07499999999999999722, 0.08749999999999999445, 0.1000000000000000056, 0.1125000000000000028, 0.1250000000000000000, 0.1375000000000000111, 0.1499999999999999944, 0.1625000000000000056, 0.1749999999999999889, 0.1875000000000000000, 0.2000000000000000111, 0.2124999999999999944, 0.2250000000000000056, 0.2374999999999999889, 0.2500000000000000000, 0.2625000000000000111, 0.2750000000000000222, 0.2874999999999999778, 0.2999999999999999889, 0.3125000000000000000, 0.3250000000000000111, 0.3375000000000000222, 0.3499999999999999778, 0.3624999999999999889, 0.3750000000000000000, 0.3875000000000000111, 0.4000000000000000222, 0.4124999999999999778, 0.4249999999999999889, 0.4375000000000000000, 0.4500000000000000111, 0.4625000000000000222, 0.4749999999999999778, 0.4874999999999999889, 0.5000000000000000000, 0.5124999999999999556, 0.5250000000000000222, 0.5374999999999999778, 0.5500000000000000444, 0.5625000000000000000, 0.5749999999999999556, 0.5875000000000000222, 0.5999999999999999778, 0.6125000000000000444, 0.6250000000000000000, 0.6374999999999999556, 0.6500000000000000222, 0.6624999999999999778, 0.6750000000000000444, 0.6875000000000000000, 0.6999999999999999556, 0.7125000000000000222, 0.7249999999999999778, 0.7375000000000000444, 0.7500000000000000000, 0.7624999999999999556, 0.7750000000000000222, 0.7874999999999999778, 0.8000000000000000444, 0.8125000000000000000, 0.8249999999999999556, 0.8375000000000000222, 0.8499999999999999778, 0.8625000000000000444, 0.8750000000000000000, 0.8874999999999999556, 0.9000000000000000222, 0.9124999999999999778, 0.9250000000000000444, 0.9375000000000000000, 0.9499999999999999556, 0.9625000000000000222, 0.9749999999999999778, 0.9875000000000000444, 1.000000000000000000 ),
 .UNSPECIFIED. ) 
 GEOMETRIC_REPRESENTATION_ITEM ( )  RATIONAL_B_SPLINE_SURFACE ( (
 ( 1.000000000000000000, 0.9238795325112867385, 1.000000000000000000, 0.9238795325112867385, 1.000000000000000000, 0.9238795325112867385, 1.000000000000000000, 0.9238795325112867385, 1.000000000000000000, 0.9238795325112867385, 1.000000000000000000, 0.9238795325112867385, 1.000000000000000000, 0.9238795325112867385, 1.000000000000000000, 0.9238795325112867385, 1.000000000000000000, 0.9238795325112867385, 1.000000000000000000, 0.9238795325112867385, 1.000000000000000000, 0.9238795325112867385, 1.000000000000000000, 0.9238795325112867385, 1.000000000000000000, 0.9238795325112867385, 1.000000000000000000, 0.9238795325112867385, 1.000000000000000000, 0.9238795325112867385, 1.000000000000000000, 0.9238795325112867385, 1.000000000000000000, 0.9238795325112867385, 1.000000000000000000, 0.9238795325112867385, 1.000000000000000000, 0.9238795325112867385, 1.000000000000000000, 0.9238795325112867385, 1.000000000000000000, 0.9238795325112867385, 1.000000000000000000, 0.9238795325112867385, 1.000000000000000000, 0.9238795325112867385, 1.000000000000000000, 0.9238795325112867385, 1.000000000000000000, 0.9238795325112867385, 1.000000000000000000, 0.9238795325112867385, 1.000000000000000000, 0.9238795325112867385, 1.000000000000000000, 0.9238795325112867385, 1.000000000000000000, 0.9238795325112867385, 1.000000000000000000, 0.9238795325112867385, 1.000000000000000000, 0.9238795325112867385, 1.000000000000000000, 0.9238795325112867385, 1.000000000000000000, 0.9238795325112867385, 1.000000000000000000, 0.9238795325112867385, 1.000000000000000000, 0.9238795325112867385, 1.000000000000000000, 0.9238795325112867385, 1.000000000000000000, 0.9238795325112867385, 1.000000000000000000, 0.9238795325112867385, 1.000000000000000000, 0.9238795325112867385, 1.000000000000000000, 0.9238795325112867385, 1.000000000000000000, 0.9238795325112867385, 1.000000000000000000, 0.9238795325112867385, 1.000000000000000000, 0.9238795325112867385, 1.000000000000000000, 0.9238795325112867385, 1.000000000000000000, 0.9238795325112867385, 1.000000000000000000, 0.9238795325112867385, 1.000000000000000000, 0.9238795325112867385, 1.000000000000000000, 0.9238795325112867385, 1.000000000000000000, 0.9238795325112867385, 1.000000000000000000, 0.9238795325112867385, 1.000000000000000000, 0.9238795325112867385, 1.000000000000000000, 0.9238795325112867385, 1.000000000000000000, 0.9238795325112867385, 1.000000000000000000, 0.9238795325112867385, 1.000000000000000000, 0.9238795325112867385, 1.000000000000000000, 0.9238795325112867385, 1.000000000000000000, 0.9238795325112867385, 1.000000000000000000, 0.9238795325112867385, 1.000000000000000000, 0.9238795325112867385, 1.000000000000000000, 0.9238795325112867385, 1.000000000000000000, 0.9238795325112867385, 1.000000000000000000, 0.9238795325112867385, 1.000000000000000000, 0.9238795325112867385, 1.000000000000000000, 0.9238795325112867385, 1.000000000000000000, 0.9238795325112867385, 1.000000000000000000, 0.9238795325112867385, 1.000000000000000000, 0.9238795325112867385, 1.000000000000000000, 0.9238795325112867385, 1.000000000000000000, 0.9238795325112867385, 1.000000000000000000, 0.9238795325112867385, 1.000000000000000000, 0.9238795325112867385, 1.000000000000000000, 0.9238795325112867385, 1.000000000000000000, 0.9238795325112867385, 1.000000000000000000, 0.9238795325112867385, 1.000000000000000000, 0.9238795325112867385, 1.000000000000000000, 0.9238795325112867385, 1.000000000000000000, 0.9238795325112867385, 1.000000000000000000, 0.9238795325112867385, 1.000000000000000000, 0.9238795325112867385, 1.000000000000000000, 0.9238795325112867385, 1.000000000000000000),
 ( 1.000000000000000000, 0.9238795325112867385, 1.000000000000000000, 0.9238795325112867385, 1.000000000000000000, 0.9238795325112867385, 1.000000000000000000, 0.9238795325112867385, 1.000000000000000000, 0.9238795325112867385, 1.000000000000000000, 0.9238795325112867385, 1.000000000000000000, 0.9238795325112867385, 1.000000000000000000, 0.9238795325112867385, 1.000000000000000000, 0.9238795325112867385, 1.000000000000000000, 0.9238795325112867385, 1.000000000000000000, 0.9238795325112867385, 1.000000000000000000, 0.9238795325112867385, 1.000000000000000000, 0.9238795325112867385, 1.000000000000000000, 0.9238795325112867385, 1.000000000000000000, 0.9238795325112867385, 1.000000000000000000, 0.9238795325112867385, 1.000000000000000000, 0.9238795325112867385, 1.000000000000000000, 0.9238795325112867385, 1.000000000000000000, 0.9238795325112867385, 1.000000000000000000, 0.9238795325112867385, 1.000000000000000000, 0.9238795325112867385, 1.000000000000000000, 0.9238795325112867385, 1.000000000000000000, 0.9238795325112867385, 1.000000000000000000, 0.9238795325112867385, 1.000000000000000000, 0.9238795325112867385, 1.000000000000000000, 0.9238795325112867385, 1.000000000000000000, 0.9238795325112867385, 1.000000000000000000, 0.9238795325112867385, 1.000000000000000000, 0.9238795325112867385, 1.000000000000000000, 0.9238795325112867385, 1.000000000000000000, 0.9238795325112867385, 1.000000000000000000, 0.9238795325112867385, 1.000000000000000000, 0.9238795325112867385, 1.000000000000000000, 0.9238795325112867385, 1.000000000000000000, 0.9238795325112867385, 1.000000000000000000, 0.9238795325112867385, 1.000000000000000000, 0.9238795325112867385, 1.000000000000000000, 0.9238795325112867385, 1.000000000000000000, 0.9238795325112867385, 1.000000000000000000, 0.9238795325112867385, 1.000000000000000000, 0.9238795325112867385, 1.000000000000000000, 0.9238795325112867385, 1.000000000000000000, 0.9238795325112867385, 1.000000000000000000, 0.9238795325112867385, 1.000000000000000000, 0.9238795325112867385, 1.000000000000000000, 0.9238795325112867385, 1.000000000000000000, 0.9238795325112867385, 1.000000000000000000, 0.9238795325112867385, 1.000000000000000000, 0.9238795325112867385, 1.000000000000000000, 0.9238795325112867385, 1.000000000000000000, 0.9238795325112867385, 1.000000000000000000, 0.9238795325112867385, 1.000000000000000000, 0.9238795325112867385, 1.000000000000000000, 0.9238795325112867385, 1.000000000000000000, 0.9238795325112867385, 1.000000000000000000, 0.9238795325112867385, 1.000000000000000000, 0.9238795325112867385, 1.000000000000000000, 0.9238795325112867385, 1.000000000000000000, 0.9238795325112867385, 1.000000000000000000, 0.9238795325112867385, 1.000000000000000000, 0.9238795325112867385, 1.000000000000000000, 0.9238795325112867385, 1.000000000000000000, 0.9238795325112867385, 1.000000000000000000, 0.9238795325112867385, 1.000000000000000000, 0.9238795325112867385, 1.000000000000000000, 0.9238795325112867385, 1.000000000000000000, 0.9238795325112867385, 1.000000000000000000, 0.9238795325112867385, 1.000000000000000000, 0.9238795325112867385, 1.000000000000000000, 0.9238795325112867385, 1.000000000000000000, 0.9238795325112867385, 1.000000000000000000, 0.9238795325112867385, 1.000000000000000000, 0.9238795325112867385, 1.000000000000000000, 0.9238795325112867385, 1.000000000000000000, 0.9238795325112867385, 1.000000000000000000, 0.9238795325112867385, 1.000000000000000000, 0.9238795325112867385, 1.000000000000000000, 0.9238795325112867385, 1.000000000000000000, 0.9238795325112867385, 1.000000000000000000, 0.9238795325112867385, 1.000000000000000000) ) ) 
 REPRESENTATION_ITEM ( '' )  SURFACE ( )  );
#15333 = CARTESIAN_POINT ( 'NONE',  ( -3.750000000000004885, 6.495190528383289141, 0.000000000000000000 ) ) ;
#15334 = DIRECTION ( 'NONE',  ( -0.000000000000000000, 1.000000000000000000, -0.000000000000000000 ) ) ;
#15335 = DIRECTION ( 'NONE',  ( -0.000000000000000000, 1.000000000000000000, -0.000000000000000000 ) ) ;
#15336 = VECTOR ( 'NONE', #2613, 1000.000000000000000 ) ;
#15337 = CARTESIAN_POINT ( 'NONE',  ( 3.535533905932738197, -22.87500000000000000, -3.535533905932738197 ) ) ;
#15338 = CARTESIAN_POINT ( 'NONE',  ( 7.500000000000004441, -4.330127018922205195, -1.000000000000000888 ) ) ;
#15339 = DIRECTION ( 'NONE',  ( 0.000000000000000000, 1.000000000000000000, -0.000000000000000000 ) ) ;
#15340 = CYLINDRICAL_SURFACE ( 'NONE', #8483, 5.000000000000001776 ) ;
#15341 = LINE ( 'NONE', #14120, #15883 ) ;
#15342 = CARTESIAN_POINT ( 'NONE',  ( 0.5093500532425063732, 4.799145180956616130, -8.374999998634409692 ) ) ;
#15343 = EDGE_LOOP ( 'NONE', ( #72, #7978, #5273, #6032 ) ) ;
#15344 = CARTESIAN_POINT ( 'NONE',  ( 0.2500000000000002220, 0.000000000000000000, 0.000000000000000000 ) ) ;
#15345 = VERTEX_POINT ( 'NONE', #15427 ) ;
#15346 = ORIENTED_EDGE ( 'NONE', *, *, #14844, .F. ) ;
#15347 = EDGE_CURVE ( 'NONE', #1547, #14832, #559, .T. ) ;
#15348 = CARTESIAN_POINT ( 'NONE',  ( -4.458734125000001214, -30.12500000136559208, 1.846868145590734089 ) ) ;
#15349 = CARTESIAN_POINT ( 'NONE',  ( -19.99999999999956657, -11.00000000000000178, 2.500000000000877520 ) ) ;
#15350 = ORIENTED_EDGE ( 'NONE', *, *, #13714, .T. ) ;
#15351 = CARTESIAN_POINT ( 'NONE',  ( -55.00000000000000000, 0.000000000000000000, -20.00000000000000711 ) ) ;
#15352 = CARTESIAN_POINT ( 'NONE',  ( 7.894705354777833861, 0.7527931906211283719, -7.590204373988224340 ) ) ;
#15353 = B_SPLINE_CURVE_WITH_KNOTS ( 'NONE', 3,
 ( #14116, #3042, #14024, #2876, #10575, #6846 ),
 .UNSPECIFIED., .F., .F.,
 ( 4, 2, 4 ),
 ( -5.145455527300660531E-06, 0.0004153350442917267738, 0.0008358155441107542345 ),
 .UNSPECIFIED. ) ;
#15354 = CARTESIAN_POINT ( 'NONE',  ( 0.5093500532425063732, 4.799145180956616130, -5.124999998634406140 ) ) ;
#15355 = CARTESIAN_POINT ( 'NONE',  ( -43.99999999999978684, -9.000000000000001776, -1.500000000000000666 ) ) ;
#15356 = CARTESIAN_POINT ( 'NONE',  ( 2.071067811865476394, -25.18750000000000000, 5.000000000000000000 ) ) ;
#15357 = CARTESIAN_POINT ( 'NONE',  ( 3.033343224707661712, -3.753672977998669946, -7.499999998634409692 ) ) ;
#15358 = CARTESIAN_POINT ( 'NONE',  ( -44.36107179304985948, -3.978804951770219756, -20.27530572909197204 ) ) ;
#15359 = DIRECTION ( 'NONE',  ( -0.000000000000000000, 1.000000000000000000, -0.000000000000000000 ) ) ;
#15360 = CARTESIAN_POINT ( 'NONE',  ( 5.000000000000000000, -26.12500000273118417, 0.000000000000000000 ) ) ;
#15361 = CARTESIAN_POINT ( 'NONE',  ( 23.49999999999956657, -8.786575603324269439E-13, -4.500000000000000000 ) ) ;
#15362 = STYLED_ITEM ( 'NONE', ( #137 ), #14078 ) ;
#15363 = CARTESIAN_POINT ( 'NONE',  ( 4.458734124999999437, -28.43750000136559564, 0.000000000000000000 ) ) ;
#15364 = CARTESIAN_POINT ( 'NONE',  ( 4.419133455865364546, -6.108866147515648493, -7.026396753507437865 ) ) ;
#15365 = ORIENTED_EDGE ( 'NONE', *, *, #12346, .F. ) ;
#15366 = ORIENTED_EDGE ( 'NONE', *, *, #227, .T. ) ;
#15368 = CARTESIAN_POINT ( 'NONE',  ( -3.401574460001765221, 4.209348295687701302, -3.562499997268815832 ) ) ;
#15367 = COLOUR_RGB ( '', 0.66274510, 0.83137255, 0.94901961) ;
#15369 = VERTEX_POINT ( 'NONE', #9205 ) ;
#15370 = CARTESIAN_POINT ( 'NONE',  ( 3.535533905932736864, -29.25000000273118772, 3.535533905932738641 ) ) ;
#15371 = ORIENTED_EDGE ( 'NONE', *, *, #3986, .F. ) ;
#15372 = DIRECTION ( 'NONE',  ( 1.000000000000000000, 0.000000000000000000, 0.000000000000000000 ) ) ;
#15373 =( GEOMETRIC_REPRESENTATION_CONTEXT ( 3 ) GLOBAL_UNCERTAINTY_ASSIGNED_CONTEXT ( ( #11265 ) ) GLOBAL_UNIT_ASSIGNED_CONTEXT ( ( #1071, #37, #12134 ) ) REPRESENTATION_CONTEXT ( 'NONE', 'WORKASPACE' ) );
#15374 = AXIS2_PLACEMENT_3D ( 'NONE', #1667, #6609, #11523 ) ;
#15375 = DIRECTION ( 'NONE',  ( -0.000000000000000000, 1.000000000000000000, -0.000000000000000000 ) ) ;
#15376 = CARTESIAN_POINT ( 'NONE',  ( 1.846868145590736310, -28.87500000136559564, 4.458734124999999437 ) ) ;
#15377 = CARTESIAN_POINT ( 'NONE',  ( 4.795541693661363958, 1.415196051561583790, -0.8749999972688139449 ) ) ;
#15378 = EDGE_CURVE ( 'NONE', #1925, #13190, #438, .T. ) ;
#15379 = CARTESIAN_POINT ( 'NONE',  ( -115.0000000000000142, -25.00000000000001066, 7.500000000000001776 ) ) ;
#15380 = CARTESIAN_POINT ( 'NONE',  ( -5.000000000000004441, -7.530481206757679743E-15, -0.5452630475929430842 ) ) ;
#15381 = ORIENTED_EDGE ( 'NONE', *, *, #13493, .F. ) ;
#15382 = MECHANICAL_DESIGN_GEOMETRIC_PRESENTATION_REPRESENTATION (  '', ( #14079 ), #15108 ) ;
#15383 =( LENGTH_UNIT ( ) NAMED_UNIT ( * ) SI_UNIT ( .MILLI., .METRE. ) );
#15384 = VERTEX_POINT ( 'NONE', #5479 ) ;
#15385 = CARTESIAN_POINT ( 'NONE',  ( -4.000000000000000000, 0.1981133338132459731, 2.096406544454392723E-17 ) ) ;
#15386 = CIRCLE ( 'NONE', #13040, 40.00000000000000711 ) ;
#15387 = ORIENTED_EDGE ( 'NONE', *, *, #5522, .T. ) ;
#15388 = VECTOR ( 'NONE', #9386, 1000.000000000000000 ) ;
#15389 = CARTESIAN_POINT ( 'NONE',  ( -4.174999999999999822, 5.112900386440199535E-16, -0.5776712190230133270 ) ) ;
#15390 = CARTESIAN_POINT ( 'NONE',  ( 2.500000000000000000, 0.000000000000000000, 0.000000000000000000 ) ) ;
#15391 = ADVANCED_FACE ( 'NONE', ( #2884 ), #8167, .F. ) ;
#15392 = CARTESIAN_POINT ( 'NONE',  ( -2.100000000000000089, 2.571758278209441957E-16, -5.000000000000000000 ) ) ;
#15393 = EDGE_CURVE ( 'NONE', #15546, #13190, #9868, .T. ) ;
#15394 = CIRCLE ( 'NONE', #13298, 5.000000000000000000 ) ;
#15395 = CARTESIAN_POINT ( 'NONE',  ( -4.799145180956616130, 0.5093500532425063732, 0.8750000013655920839 ) ) ;
#15396 = FACE_OUTER_BOUND ( 'NONE', #1851, .T. ) ;
#15397 = LINE ( 'NONE', #10625, #11060 ) ;
#15398 = FACE_OUTER_BOUND ( 'NONE', #14014, .T. ) ;
#15399 = ORIENTED_EDGE ( 'NONE', *, *, #8907, .F. ) ;
#15400 = CARTESIAN_POINT ( 'NONE',  ( 7.500000000000000888, 3.988838049906433092, -0.8529248949437668870 ) ) ;
#15401 = LINE ( 'NONE', #3025, #1198 ) ;
#15402 = DIRECTION ( 'NONE',  ( -0.000000000000000000, -0.000000000000000000, -1.000000000000000000 ) ) ;
#15403 = EDGE_LOOP ( 'NONE', ( #4106, #4712, #14754, #3100 ) ) ;
#15404 = CARTESIAN_POINT ( 'NONE',  ( 39.53738644056090124, -5.000000000000000000, 28.48076211354432985 ) ) ;
#15405 = VECTOR ( 'NONE', #9395, 1000.000000000000000 ) ;
#15406 = ORIENTED_EDGE ( 'NONE', *, *, #10715, .T. ) ;
#15407 = ORIENTED_EDGE ( 'NONE', *, *, #13846, .T. ) ;
#15408 = DIRECTION ( 'NONE',  ( 0.000000000000000000, -1.000000000000000000, 0.000000000000000000 ) ) ;
#15409 = CARTESIAN_POINT ( 'NONE',  ( -0.5469614295416921346, 4.303013824936271270, -3.535263753543735454 ) ) ;
#15410 = VECTOR ( 'NONE', #4486, 1000.000000000000000 ) ;
#15411 = DIRECTION ( 'NONE',  ( 0.000000000000000000, 0.000000000000000000, 1.000000000000000000 ) ) ;
#15412 = AXIS2_PLACEMENT_3D ( 'NONE', #14906, #2602, #5123 ) ;
#15413 = ADVANCED_FACE ( 'NONE', ( #6775 ), #10258, .T. ) ;
#15414 = CARTESIAN_POINT ( 'NONE',  ( 3.061616997868383141E-16, -25.87500000273118417, -5.000000000000000000 ) ) ;
#15416 = DIRECTION ( 'NONE',  ( 0.000000000000000000, 1.000000000000000000, 0.000000000000000000 ) ) ;
#15415 = VECTOR ( 'NONE', #12218, 1000.000000000000000 ) ;
#15417 = EDGE_CURVE ( 'NONE', #11644, #6256, #6534, .T. ) ;
#15418 = CARTESIAN_POINT ( 'NONE',  ( -124.9999999999999716, -10.00000000000001066, -7.500000000000000000 ) ) ;
#15419 = PRODUCT_DEFINITION_SHAPE ( 'NONE', 'NONE',  #15989 ) ;
#15420 = FACE_OUTER_BOUND ( 'NONE', #3353, .T. ) ;
#15421 = DIRECTION ( 'NONE',  ( 0.000000000000000000, 0.000000000000000000, -1.000000000000000000 ) ) ;
#15422 = CARTESIAN_POINT ( 'NONE',  ( 0.000000000000000000, 40.00000000000000000, 25.00000000000000000 ) ) ;
#15423 = CARTESIAN_POINT ( 'NONE',  ( -1.846868145590737420, -29.00000000136559564, 4.458734124999997661 ) ) ;
#15424 = CONICAL_SURFACE ( 'NONE', #9004, 2.055000000000000160, 0.7853981633974633780 ) ;
#15425 = CARTESIAN_POINT ( 'NONE',  ( -3.033343224707664376, 3.753672977998667726, 1.365593156898739876E-09 ) ) ;
#15426 = VERTEX_POINT ( 'NONE', #4180 ) ;
#15427 = CARTESIAN_POINT ( 'NONE',  ( 35.00000000000000000, 40.00000000000000000, -2.649999999999992806 ) ) ;
#15428 = VERTEX_POINT ( 'NONE', #5316 ) ;
#15429 = VERTEX_POINT ( 'NONE', #15183 ) ;
#15430 =( BOUNDED_CURVE ( )  B_SPLINE_CURVE ( 3, ( #1570, #1496, #12549, #10227 ),
 .UNSPECIFIED., .F., .F. ) 
 B_SPLINE_CURVE_WITH_KNOTS ( ( 4, 4 ),
 ( 1.570796326794896780, 3.141592653589793116 ),
 .UNSPECIFIED. ) 
 CURVE ( )  GEOMETRIC_REPRESENTATION_ITEM ( )  RATIONAL_B_SPLINE_CURVE ( ( 1.000000000000000000, 0.8047378541243650485, 0.8047378541243650485, 1.000000000000000000 ) ) 
 REPRESENTATION_ITEM ( '' )  );
#15431 = SURFACE_STYLE_USAGE ( .BOTH. , #2583 ) ;
#15432 = CARTESIAN_POINT ( 'NONE',  ( -4.458734125000001214, -27.12500000136559564, 1.846868145590734089 ) ) ;
#15433 = DIRECTION ( 'NONE',  ( -0.000000000000000000, 1.000000000000000000, -0.000000000000000000 ) ) ;
#15434 = AXIS2_PLACEMENT_3D ( 'NONE', #1397, #7562, #122 ) ;
#15435 = EDGE_LOOP ( 'NONE', ( #8921, #4796, #5384, #14383 ) ) ;
#15436 = CARTESIAN_POINT ( 'NONE',  ( -0.5711823568785977523, -5.381735091635034607, -6.312500000000000000 ) ) ;
#15437 = AXIS2_PLACEMENT_3D ( 'NONE', #13405, #9617, #1129 ) ;
#15438 = CARTESIAN_POINT ( 'NONE',  ( 7.500000000000000000, 1.572594658376105459, -7.069792055233640404 ) ) ;
#15439 = EDGE_CURVE ( 'NONE', #637, #9381, #4465, .T. ) ;
#15440 = CARTESIAN_POINT ( 'NONE',  ( -3.753672977998669502, -3.033343224707661712, -5.749999998634407916 ) ) ;
#15441 = CARTESIAN_POINT ( 'NONE',  ( 14.41154273188008439, 88.59290746114278647, 60.96152422706632024 ) ) ;
#15442 = ADVANCED_FACE ( 'NONE', ( #14035 ), #2960, .T. ) ;
#15443 = CARTESIAN_POINT ( 'NONE',  ( -2.071067811865478170, -24.31250000000000000, 5.000000000000000000 ) ) ;
#15444 = CARTESIAN_POINT ( 'NONE',  ( -4.276409079477644148, -1.261996585732578335, -6.812499998634407028 ) ) ;
#15445 = CARTESIAN_POINT ( 'NONE',  ( -9.184850993605147944E-16, -21.37500000273118772, 5.000000000000000000 ) ) ;
#15446 = CIRCLE ( 'NONE', #14142, 4.250000000000000000 ) ;
#15447 = CARTESIAN_POINT ( 'NONE',  ( 35.00000000000000000, 50.00000000000000000, 0.000000000000000000 ) ) ;
#15448 = CARTESIAN_POINT ( 'NONE',  ( 3.061616997868383141E-16, -25.87500000273118417, -5.000000000000000000 ) ) ;
#15449 = AXIS2_PLACEMENT_3D ( 'NONE', #11249, #196, #5194 ) ;
#15450 = ORIENTED_EDGE ( 'NONE', *, *, #11333, .T. ) ;
#15451 = CARTESIAN_POINT ( 'NONE',  ( 4.458734124999997661, -27.50000000136559564, 1.846868145590737864 ) ) ;
#15452 = CARTESIAN_POINT ( 'NONE',  ( 0.9763930676203995684, -8.096533237418878315, -7.213065638943601421 ) ) ;
#15453 = EDGE_LOOP ( 'NONE', ( #7520, #2054, #5975, #15285 ) ) ;
#15454 = ORIENTED_EDGE ( 'NONE', *, *, #6802, .F. ) ;
#15455 = AXIS2_PLACEMENT_3D ( 'NONE', #13744, #2676, #6418 ) ;
#15456 = DIRECTION ( 'NONE',  ( -0.8660254037844383745, 0.000000000000000000, -0.5000000000000004441 ) ) ;
#15457 = ORIENTED_EDGE ( 'NONE', *, *, #6840, .F. ) ;
#15458 = CARTESIAN_POINT ( 'NONE',  ( 30.02221399786055400, 0.000000000000000000, -15.99999999999999645 ) ) ;
#15459 = VECTOR ( 'NONE', #14852, 1000.000000000000000 ) ;
#15460 = PRODUCT ( 'socket head cap screw_iso_ISO 4762 M5 x 20 - 20N', 'socket head cap screw_iso_ISO 4762 M5 x 20 - 20N', '', ( #5267 ) ) ;
#15461 = CARTESIAN_POINT ( 'NONE',  ( 39.90991147063509459, -3.660959011663038609, -28.10869455183395971 ) ) ;
#15462 = EDGE_CURVE ( 'NONE', #11118, #8118, #5640, .T. ) ;
#15463 = CARTESIAN_POINT ( 'NONE',  ( 3.152801135295366208, -25.81250000136559564, 3.152801135295367985 ) ) ;
#15464 = CIRCLE ( 'NONE', #14423, 9.999999999999994671 ) ;
#15465 = CARTESIAN_POINT ( 'NONE',  ( -0.5711823568785977523, -5.381735091635034607, -4.312499999999999112 ) ) ;
#15466 = ITEM_DEFINED_TRANSFORMATION ( 'NONE', 'NONE', #13507,  #3223 ) ;
#15467 = CARTESIAN_POINT ( 'NONE',  ( -3.916244202832140253, 2.131511515620587272, -8.187499998634407916 ) ) ;
#15468 = CARTESIAN_POINT ( 'NONE',  ( -4.799145180956616130, 0.5093500532425063732, -0.1249999986344088321 ) ) ;
#15469 = ORIENTED_EDGE ( 'NONE', *, *, #12323, .F. ) ;
#15470 = CIRCLE ( 'NONE', #10568, 2.041999999999999815 ) ;
#15471 = ORIENTED_EDGE ( 'NONE', *, *, #9644, .T. ) ;
#15472 = ADVANCED_FACE ( 'NONE', ( #5954 ), #4423, .F. ) ;
#15473 = CARTESIAN_POINT ( 'NONE',  ( -4.599534470797605579, 6.460478697737046971, -7.590212325761443779 ) ) ;
#15474 = AXIS2_PLACEMENT_3D ( 'NONE', #15758, #6127, #2157 ) ;
#15475 = ORIENTED_EDGE ( 'NONE', *, *, #673, .T. ) ;
#15476 = ITEM_DEFINED_TRANSFORMATION ( 'NONE', 'NONE', #10452,  #3223 ) ;
#15477 = ADVANCED_FACE ( 'NONE', ( #15508 ), #13826, .T. ) ;
#15478 = CARTESIAN_POINT ( 'NONE',  ( 2.390265326283148806, 4.391654775818395251, -4.875000000000000888 ) ) ;
#15479 = CARTESIAN_POINT ( 'NONE',  ( 0.000000000000000000, 0.000000000000000000, 0.000000000000000000 ) ) ;
#15480 = LINE ( 'NONE', #683, #13332 ) ;
#15481 = CARTESIAN_POINT ( 'NONE',  ( -4.391654775818395251, 2.390265326283148806, -7.499999997268816720 ) ) ;
#15482 = CARTESIAN_POINT ( 'NONE',  ( -5.000000000000004441, -7.530481206757679743E-15, -0.5452630475929430842 ) ) ;
#15483 = FACE_OUTER_BOUND ( 'NONE', #12053, .T. ) ;
#15484 = ORIENTED_EDGE ( 'NONE', *, *, #4144, .F. ) ;
#15485 = DIRECTION ( 'NONE',  ( 0.000000000000000000, 1.000000000000000000, 0.000000000000000000 ) ) ;
#15486 = CARTESIAN_POINT ( 'NONE',  ( -1.415196051561583790, 4.795541693661363958, -2.624999997268815388 ) ) ;
#15487 = DIRECTION ( 'NONE',  ( 0.000000000000000000, 0.000000000000000000, 1.000000000000000000 ) ) ;
#15488 = ORIENTED_EDGE ( 'NONE', *, *, #7135, .T. ) ;
#15489 = CARTESIAN_POINT ( 'NONE',  ( -6.765421556309547668E-13, 50.00000000000000000, 67.49999999999930367 ) ) ;
#15490 = ORIENTED_EDGE ( 'NONE', *, *, #4846, .F. ) ;
#15491 = ORIENTED_EDGE ( 'NONE', *, *, #799, .F. ) ;
#15492 = CARTESIAN_POINT ( 'NONE',  ( 27.49999999999998224, -5.000000000000000000, 47.63139720814412925 ) ) ;
#15493 = EDGE_CURVE ( 'NONE', #1764, #362, #2991, .T. ) ;
#15494 = DIRECTION ( 'NONE',  ( 0.000000000000000000, 0.000000000000000000, 1.000000000000000000 ) ) ;
#15495 = EDGE_CURVE ( 'NONE', #7134, #434, #6943, .T. ) ;
#15496 = CARTESIAN_POINT ( 'NONE',  ( -115.2406606923551919, -116.0588903632565518, -17.49999999999999645 ) ) ;
#15497 =( REPRESENTATION_RELATIONSHIP ('NONE','NONE', #4176, #15130 ) REPRESENTATION_RELATIONSHIP_WITH_TRANSFORMATION ( #751 )SHAPE_REPRESENTATION_RELATIONSHIP( ) );
#15498 = LINE ( 'NONE', #15571, #7939 ) ;
#15499 = CARTESIAN_POINT ( 'NONE',  ( -2.071067811865492381, -25.31250000000000000, 4.999999999999985789 ) ) ;
#15500 = CARTESIAN_POINT ( 'NONE',  ( 0.000000000000000000, 2.000000000000001776, 0.000000000000000000 ) ) ;
#15501 = CARTESIAN_POINT ( 'NONE',  ( 0.000000000000000000, 0.000000000000000000, -5.000000000000000000 ) ) ;
#15502 = DIRECTION ( 'NONE',  ( 0.000000000000000000, 0.000000000000000000, -1.000000000000000000 ) ) ;
#15503 = DIRECTION ( 'NONE',  ( -1.000000000000000000, -0.000000000000000000, -0.000000000000000000 ) ) ;
#15504 = CARTESIAN_POINT ( 'NONE',  ( -4.458734124999999437, -31.18750000136559564, -5.460374474430324690E-16 ) ) ;
#15505 = CARTESIAN_POINT ( 'NONE',  ( 2.131511515620586383, 3.916244202832140253, -1.187499998634405918 ) ) ;
#15506 = VERTEX_POINT ( 'NONE', #716 ) ;
#15507 = UNCERTAINTY_MEASURE_WITH_UNIT (LENGTH_MEASURE( 1.000000000000000082E-05 ), #15700, 'distance_accuracy_value', 'NONE');
#15508 = FACE_OUTER_BOUND ( 'NONE', #5121, .T. ) ;
#15509 = ORIENTED_EDGE ( 'NONE', *, *, #5993, .F. ) ;
#15510 = ORIENTED_EDGE ( 'NONE', *, *, #2217, .F. ) ;
#15511 = FILL_AREA_STYLE ('',( #2746 ) ) ;
#15512 = CARTESIAN_POINT ( 'NONE',  ( -8.190561711645485556E-16, -28.93750000136559564, 4.458734124999999437 ) ) ;
#15513 = CARTESIAN_POINT ( 'NONE',  ( -45.00000000000000000, 0.000000000000000000, 7.500000000000001776 ) ) ;
#15514 = EDGE_CURVE ( 'NONE', #2381, #15134, #12777, .T. ) ;
#15515 = CARTESIAN_POINT ( 'NONE',  ( -28.86751345948126612, -37.00000000000000711, -20.00000000000000355 ) ) ;
#15516 = CARTESIAN_POINT ( 'NONE',  ( 7.499999999999650946, 0.7577384720642122984, -7.446470314338120566 ) ) ;
#15517 = CARTESIAN_POINT ( 'NONE',  ( 1.261996585732578113, -4.276409079477644148, -4.562499998634405252 ) ) ;
#15518 = CARTESIAN_POINT ( 'NONE',  ( 3.518113437216164652, -3.097286126993894495, 48.83433521136175415 ) ) ;
#15519 = CARTESIAN_POINT ( 'NONE',  ( -5.000000000000000888, -24.56250000000000000, -2.071067811865475949 ) ) ;
#15520 = CARTESIAN_POINT ( 'NONE',  ( 3.033343224707661712, -3.753672977998669946, -6.499999998634407916 ) ) ;
#15521 = CARTESIAN_POINT ( 'NONE',  ( -55.00000000000000000, -10.00000000000000178, -17.50000000000000000 ) ) ;
#15522 = CARTESIAN_POINT ( 'NONE',  ( 5.000000000000000888, 0.000000000000000000, -25.03750572909317285 ) ) ;
#15523 = CARTESIAN_POINT ( 'NONE',  ( 3.535533905932736864, -21.25000000273118772, 3.535533905932738641 ) ) ;
#15524 = ORIENTED_EDGE ( 'NONE', *, *, #7812, .T. ) ;
#15525 = CARTESIAN_POINT ( 'NONE',  ( -8.190561711645485556E-16, -21.68750000136559208, 4.458734124999999437 ) ) ;
#15526 = CARTESIAN_POINT ( 'NONE',  ( -1.415196051561583790, 4.795541693661363958, -6.750000000000002665 ) ) ;
#15527 = ORIENTED_EDGE ( 'NONE', *, *, #15905, .T. ) ;
#15528 = ORIENTED_EDGE ( 'NONE', *, *, #6192, .T. ) ;
#15529 = CARTESIAN_POINT ( 'NONE',  ( -60.00000000000000000, -37.00000000000000711, -20.00000000000000711 ) ) ;
#15530 = EDGE_CURVE ( 'NONE', #7701, #9678, #7092, .T. ) ;
#15531 = CARTESIAN_POINT ( 'NONE',  ( 3.061616997868383141E-16, -28.87500000273118772, -5.000000000000000000 ) ) ;
#15532 = EDGE_CURVE ( 'NONE', #13331, #9071, #14283, .T. ) ;
#15533 = ADVANCED_FACE ( 'NONE', ( #8154 ), #11845, .F. ) ;
#15534 = ADVANCED_FACE ( 'NONE', ( #5713 ), #5830, .F. ) ;
#15535 = VERTEX_POINT ( 'NONE', #1022 ) ;
#15536 = DIRECTION ( 'NONE',  ( 0.000000000000000000, 0.000000000000000000, 1.000000000000000000 ) ) ;
#15537 = CARTESIAN_POINT ( 'NONE',  ( 6.000000000000000000, -13.00000000000000178, 1.500000000000000000 ) ) ;
#15538 = CARTESIAN_POINT ( 'NONE',  ( -4.458734125000000326, -28.25000000136559208, -1.846868145590735644 ) ) ;
#15539 = CARTESIAN_POINT ( 'NONE',  ( 2.875844205641825191, -3.000000000000000000, -48.98110827882413787 ) ) ;
#15540 = CARTESIAN_POINT ( 'NONE',  ( 67.49999999999931788, 37.00000000000000000, 2.081668171172168513E-14 ) ) ;
#15541 = DIRECTION ( 'NONE',  ( 0.000000000000000000, 0.000000000000000000, 1.000000000000000000 ) ) ;
#15542 = FACE_OUTER_BOUND ( 'NONE', #2097, .T. ) ;
#15543 = CARTESIAN_POINT ( 'NONE',  ( 4.276409079477644148, 1.261996585732577891, -0.5624999986344088043 ) ) ;
#15544 = EDGE_LOOP ( 'NONE', ( #15122, #206, #11607, #14149 ) ) ;
#15545 = PRODUCT_CONTEXT ( 'NONE', #9798, 'mechanical' ) ;
#15546 = VERTEX_POINT ( 'NONE', #4733 ) ;
#15547 = CARTESIAN_POINT ( 'NONE',  ( 30.02221399786053979, 88.59290746114278647, -15.99999999999998579 ) ) ;
#15548 = EDGE_CURVE ( 'NONE', #3191, #15584, #6355, .T. ) ;
#15549 = ORIENTED_EDGE ( 'NONE', *, *, #1759, .T. ) ;
#15550 = ITEM_DEFINED_TRANSFORMATION ( 'NONE', 'NONE', #957,  #3223 ) ;
#15551 = B_SPLINE_CURVE_WITH_KNOTS ( 'NONE', 3,
 ( #4807, #5945, #12145, #8306, #13197, #11982 ),
 .UNSPECIFIED., .F., .F.,
 ( 4, 2, 4 ),
 ( 0.004615310220740751271, 0.006918661718823357169, 0.009222013216905963068 ),
 .UNSPECIFIED. ) ;
#15552 = DIRECTION ( 'NONE',  ( -0.000000000000000000, -1.000000000000000000, -0.000000000000000000 ) ) ;
#15553 = CARTESIAN_POINT ( 'NONE',  ( 19.99999999999956657, -8.786575603324269439E-13, 0.000000000000000000 ) ) ;
#15554 = CARTESIAN_POINT ( 'NONE',  ( 1.655952806101427033, -3.662737355149048302, -1.182683869819604841E-14 ) ) ;
#15555 = CARTESIAN_POINT ( 'NONE',  ( -2.131511515620587272, -3.916244202832140253, 1.062500001365592528 ) ) ;
#15556 = DIRECTION ( 'NONE',  ( -0.000000000000000000, -1.000000000000000000, -0.000000000000000000 ) ) ;
#15557 = CARTESIAN_POINT ( 'NONE',  ( -4.211140560182196957, -2.431303136016552013, -3.745885042887436178 ) ) ;
#15558 = CARTESIAN_POINT ( 'NONE',  ( 2.500000000000000000, 2.357898499370433054, -1.951563910473907981E-15 ) ) ;
#15559 = ORIENTED_EDGE ( 'NONE', *, *, #4233, .T. ) ;
#15560 = CARTESIAN_POINT ( 'NONE',  ( -31.74999999999995737, 0.000000000000000000, 4.250000000000000000 ) ) ;
#15561 = CARTESIAN_POINT ( 'NONE',  ( -4.999999999999849898, 1.272547481429008309, -2.461597479913463893 ) ) ;
#15562 = CARTESIAN_POINT ( 'NONE',  ( -90.00000000000000000, -35.00000000000000711, 7.500000000000001776 ) ) ;
#15563 = VERTEX_POINT ( 'NONE', #10953 ) ;
#15564 = CARTESIAN_POINT ( 'NONE',  ( 2.071067811865461294, -26.81249999999999289, -5.000000000000014211 ) ) ;
#15565 = ORIENTED_EDGE ( 'NONE', *, *, #8773, .T. ) ;
#15566 = VECTOR ( 'NONE', #9854, 1000.000000000000114 ) ;
#15567 = ORIENTED_EDGE ( 'NONE', *, *, #2316, .F. ) ;
#15568 = CARTESIAN_POINT ( 'NONE',  ( 0.000000000000000000, -20.00000000000000000, 0.000000000000000000 ) ) ;
#15569 = CARTESIAN_POINT ( 'NONE',  ( -67.50000000000000000, 37.00000000000000000, -7.070249711157346244E-13 ) ) ;
#15570 = PLANE ( 'NONE',  #4249 ) ;
#15571 = CARTESIAN_POINT ( 'NONE',  ( 3.164319481612644314, -3.000000000000000000, 49.48076211353313880 ) ) ;
#15572 = CARTESIAN_POINT ( 'NONE',  ( 2.467663300281916943E-15, 40.00000000000000000, -64.85000000000000853 ) ) ;
#15573 = DIRECTION ( 'NONE',  ( 0.000000000000000000, 0.000000000000000000, -1.000000000000000000 ) ) ;
#15574 = CYLINDRICAL_SURFACE ( 'NONE', #13359, 2.649999999999999467 ) ;
#15575 = ADVANCED_FACE ( 'NONE', ( #7491 ), #2456, .T. ) ;
#15576 = VECTOR ( 'NONE', #2733, 1000.000000000000000 ) ;
#15577 = CARTESIAN_POINT ( 'NONE',  ( -81.33974596215560382, -110.0591436588189538, 7.500000000000001776 ) ) ;
#15578 = ADVANCED_FACE ( 'NONE', ( #8703 ), #1090, .T. ) ;
#15579 = CARTESIAN_POINT ( 'NONE',  ( -3.152801135295367096, -30.31250000136559564, -3.152801135295367541 ) ) ;
#15580 = CARTESIAN_POINT ( 'NONE',  ( -3.033343224707664376, 3.753672977998667726, -1.999999998634408360 ) ) ;
#15581 = ORIENTED_EDGE ( 'NONE', *, *, #9103, .T. ) ;
#15582 = CARTESIAN_POINT ( 'NONE',  ( 6.523606932381143864, 4.893847819346820671, -7.213065638944192060 ) ) ;
#15583 = EDGE_LOOP ( 'NONE', ( #2538, #2558, #12468, #4055, #13027 ) ) ;
#15584 = VERTEX_POINT ( 'NONE', #12394 ) ;
#15585 = PRODUCT_DEFINITION_SHAPE ( 'NONE', 'NONE',  #12418 ) ;
#15586 = CARTESIAN_POINT ( 'NONE',  ( -8.190561711645485556E-16, -25.93750000136559564, 4.458734124999999437 ) ) ;
#15587 = LINE ( 'NONE', #5717, #5332 ) ;
#15588 = CARTESIAN_POINT ( 'NONE',  ( -4.209348295687703079, -3.401574460001763445, -6.437500000000003553 ) ) ;
#15589 = CARTESIAN_POINT ( 'NONE',  ( 3.061616997868383141E-16, -29.75000000000000000, -5.000000000000000000 ) ) ;
#15590 = CARTESIAN_POINT ( 'NONE',  ( 0.5093500532425063732, 4.799145180956616130, -6.124999998634407916 ) ) ;
#15591 = CARTESIAN_POINT ( 'NONE',  ( 2.143131898507869826E-15, 50.00000000000000000, -67.50000000000000000 ) ) ;
#15592 = CARTESIAN_POINT ( 'NONE',  ( 3.535533905932736864, -27.12500000000000000, 3.535533905932738641 ) ) ;
#15593 = CARTESIAN_POINT ( 'NONE',  ( -4.799145180956616130, 0.5093500532425063732, -6.874999998634407916 ) ) ;
#15594 = LINE ( 'NONE', #4591, #5784 ) ;
#15595 = ADVANCED_FACE ( 'NONE', ( #2377 ), #2209, .T. ) ;
#15596 = CARTESIAN_POINT ( 'NONE',  ( 16.49999999999956657, -8.786575603324269439E-13, 0.000000000000000000 ) ) ;
#15597 = EDGE_CURVE ( 'NONE', #15267, #12836, #9984, .T. ) ;
#15598 = CARTESIAN_POINT ( 'NONE',  ( 3.535533905932738197, -22.00000000273118772, -3.535533905932738197 ) ) ;
#15599 = ORIENTED_EDGE ( 'NONE', *, *, #4707, .T. ) ;
#15600 = CARTESIAN_POINT ( 'NONE',  ( -8.190561711645485556E-16, -22.68750000136559564, 4.458734124999999437 ) ) ;
#15601 = CARTESIAN_POINT ( 'NONE',  ( -21.01110699893041911, 0.000000000000000000, -33.74230484541335073 ) ) ;
#15602 = ORIENTED_EDGE ( 'NONE', *, *, #9869, .F. ) ;
#15603 = VERTEX_POINT ( 'NONE', #2309 ) ;
#15604 = CARTESIAN_POINT ( 'NONE',  ( 3.061616997868383141E-16, -22.75000000000000000, -5.000000000000000000 ) ) ;
#15605 = CARTESIAN_POINT ( 'NONE',  ( 1.846868145590736310, -27.62500000136559564, 4.458734124999999437 ) ) ;
#15606 = CARTESIAN_POINT ( 'NONE',  ( 3.401574460001763445, -4.209348295687703079, -7.062499997268814944 ) ) ;
#15607 = CIRCLE ( 'NONE', #11963, 2.000000000000000888 ) ;
#15608 = ORIENTED_EDGE ( 'NONE', *, *, #7478, .T. ) ;
#15609 = CARTESIAN_POINT ( 'NONE',  ( -5.000000000000000000, -24.62500000273118417, -6.123233995736766282E-16 ) ) ;
#15610 = CARTESIAN_POINT ( 'NONE',  ( 40.36046224127503024, -3.194220869028281395, -27.64520767097959819 ) ) ;
#15611 = CARTESIAN_POINT ( 'NONE',  ( 3.152801135295367541, -28.56250000136559564, -3.152801135295367541 ) ) ;
#15612 = AXIS2_PLACEMENT_3D ( 'NONE', #12129, #11889, #9628 ) ;
#15613 = DIRECTION ( 'NONE',  ( 0.000000000000000000, -1.000000000000000000, 0.000000000000000000 ) ) ;
#15614 = ADVANCED_FACE ( 'NONE', ( #7574 ), #11189, .F. ) ;
#15615 = CARTESIAN_POINT ( 'NONE',  ( -5.000000000000095035, -0.7223674278660573433, -4.521799365517152225 ) ) ;
#15616 = EDGE_CURVE ( 'NONE', #7457, #4101, #13688, .T. ) ;
#15617 = SURFACE_STYLE_FILL_AREA ( #10912 ) ;
#15618 = AXIS2_PLACEMENT_3D ( 'NONE', #3852, #8951, #13863 ) ;
#15619 = FACE_OUTER_BOUND ( 'NONE', #10284, .T. ) ;
#15620 = ORIENTED_EDGE ( 'NONE', *, *, #846, .T. ) ;
#15621 = SURFACE_SIDE_STYLE ('',( #7797 ) ) ;
#15622 = ORIENTED_EDGE ( 'NONE', *, *, #2570, .T. ) ;
#15623 = CARTESIAN_POINT ( 'NONE',  ( -6.625705691649780960, 5.306270977113050513, -7.795653906408979594 ) ) ;
#15624 = AXIS2_PLACEMENT_3D ( 'NONE', #11823, #4480, #3416 ) ;
#15625 = CIRCLE ( 'NONE', #10714, 3.499999999999999556 ) ;
#15626 = VERTEX_POINT ( 'NONE', #5054 ) ;
#15627 = MECHANICAL_DESIGN_GEOMETRIC_PRESENTATION_REPRESENTATION (  '', ( #12508 ), #4268 ) ;
#15628 = DIRECTION ( 'NONE',  ( 0.000000000000000000, 0.000000000000000000, -1.000000000000000000 ) ) ;
#15629 = CARTESIAN_POINT ( 'NONE',  ( -7.500000000000005329, 4.330127018922194537, -7.422398894150031623 ) ) ;
#15630 = CARTESIAN_POINT ( 'NONE',  ( 2.131511515620586383, 3.916244202832140253, 0.8125000013655924169 ) ) ;
#15631 = CARTESIAN_POINT ( 'NONE',  ( 1.836970198721031955E-15, 32.00000000000000000, -67.50000000000000000 ) ) ;
#15632 = EDGE_CURVE ( 'NONE', #7177, #7141, #15083, .T. ) ;
#15633 = VECTOR ( 'NONE', #14947, 1000.000000000000000 ) ;
#15634 = CARTESIAN_POINT ( 'NONE',  ( -0.5093500532425060401, -4.799145180956616130, -0.8749999986344056957 ) ) ;
#15635 = CARTESIAN_POINT ( 'NONE',  ( 2.390265326283148806, 4.391654775818395251, -0.8750000000000007772 ) ) ;
#15636 = CARTESIAN_POINT ( 'NONE',  ( 2.500000000000000000, -2.357898499370432610, 3.252606517456513302E-15 ) ) ;
#15637 = ORIENTED_EDGE ( 'NONE', *, *, #226, .T. ) ;
#15638 = CIRCLE ( 'NONE', #12265, 2.000000000000001776 ) ;
#15639 = DIRECTION ( 'NONE',  ( 0.000000000000000000, -1.000000000000000000, 0.000000000000000000 ) ) ;
#15640 = DIRECTION ( 'NONE',  ( -0.000000000000000000, 1.000000000000000000, -0.000000000000000000 ) ) ;
#15641 = CARTESIAN_POINT ( 'NONE',  ( -91.28042740779480368, -120.0589677227266918, 17.50000000000000000 ) ) ;
#15642 = ORIENTED_EDGE ( 'NONE', *, *, #5540, .F. ) ;
#15643 = CARTESIAN_POINT ( 'NONE',  ( 16.49999999999956657, -8.782289339527253835E-13, -11.50000000000000000 ) ) ;
#15644 = VERTEX_POINT ( 'NONE', #2619 ) ;
#15645 = EDGE_LOOP ( 'NONE', ( #15325, #1562, #14207, #5056 ) ) ;
#15646 = CARTESIAN_POINT ( 'NONE',  ( 3.033343224707661712, -3.753672977998669502, -0.7499999986344074721 ) ) ;
#15647 = FACE_OUTER_BOUND ( 'NONE', #11628, .T. ) ;
#15648 = FILL_AREA_STYLE_COLOUR ( '', #15367 ) ;
#15649 = VECTOR ( 'NONE', #8731, 1000.000000000000000 ) ;
#15650 = PLANE ( 'NONE',  #11785 ) ;
#15651 = CARTESIAN_POINT ( 'NONE',  ( 35.00000000000000000, 37.00000000000000000, -8.572527594031472993E-15 ) ) ;
#15652 = EDGE_CURVE ( 'NONE', #7272, #9435, #5315, .T. ) ;
#15653 = DIRECTION ( 'NONE',  ( 0.000000000000000000, 1.000000000000000000, 0.000000000000000000 ) ) ;
#15654 = CARTESIAN_POINT ( 'NONE',  ( 4.795541693661363958, 1.415196051561583790, -8.000000000000003553 ) ) ;
#15655 = DIRECTION ( 'NONE',  ( 0.000000000000000000, -0.5000000000000011102, -0.8660254037844379305 ) ) ;
#15656 = CARTESIAN_POINT ( 'NONE',  ( 3.152801135295366208, -29.81250000136559208, 3.152801135295367985 ) ) ;
#15657 =( BOUNDED_CURVE ( )  B_SPLINE_CURVE ( 2, ( #6252, #3655, #2427, #108, #5027, #9957, #13665, #2595, #7549 ),
 .UNSPECIFIED., .F., .F. ) 
 B_SPLINE_CURVE_WITH_KNOTS ( ( 3, 2, 2, 2, 3 ),
 ( 0.7750000000000000222, 0.7874999999999999778, 0.8000000000000000444, 0.8125000000000001110, 0.8250000000000000666 ),
 .UNSPECIFIED. ) 
 CURVE ( )  GEOMETRIC_REPRESENTATION_ITEM ( )  RATIONAL_B_SPLINE_CURVE ( ( 1.000000000000000000, 0.9238795325112867385, 1.000000000000000000, 0.9238795325112867385, 1.000000000000000000, 0.9238795325112867385, 1.000000000000000000, 0.9238795325112860723, 1.000000000000000666 ) ) 
 REPRESENTATION_ITEM ( '' )  );
#15658 = CARTESIAN_POINT ( 'NONE',  ( -3.916244202832140253, 2.131511515620587272, -0.9374999986344056957 ) ) ;
#15659 = ORIENTED_EDGE ( 'NONE', *, *, #400, .T. ) ;
#15660 =( GEOMETRIC_REPRESENTATION_CONTEXT ( 3 ) GLOBAL_UNCERTAINTY_ASSIGNED_CONTEXT ( ( #607 ) ) GLOBAL_UNIT_ASSIGNED_CONTEXT ( ( #5032, #9719, #3583 ) ) REPRESENTATION_CONTEXT ( 'NONE', 'WORKASPACE' ) );
#15661 = CARTESIAN_POINT ( 'NONE',  ( 3.093533885182924159, 6.874201416486802607, -7.446478553994766436 ) ) ;
#15662 = ORIENTED_EDGE ( 'NONE', *, *, #2599, .T. ) ;
#15663 = ORIENTED_EDGE ( 'NONE', *, *, #3366, .F. ) ;
#15664 = AXIS2_PLACEMENT_3D ( 'NONE', #14842, #1260, #4977 ) ;
#15665 = ORIENTED_EDGE ( 'NONE', *, *, #1640, .T. ) ;
#15666 = AXIS2_PLACEMENT_3D ( 'NONE', #9638, #11101, #3736 ) ;
#15667 = CARTESIAN_POINT ( 'NONE',  ( 2.730187237215162345E-16, -25.43750000136559564, -4.458734124999999437 ) ) ;
#15668 = FACE_OUTER_BOUND ( 'NONE', #2934, .T. ) ;
#15669 = CARTESIAN_POINT ( 'NONE',  ( -35.00000000000000000, 37.00000000000000000, 6.000000000000000000 ) ) ;
#15670 = ADVANCED_FACE ( 'NONE', ( #8622 ), #13515, .F. ) ;
#15671 = VECTOR ( 'NONE', #14526, 1000.000000000000000 ) ;
#15672 = CARTESIAN_POINT ( 'NONE',  ( 4.276409079477644148, 1.261996585732577891, -7.312499998634407916 ) ) ;
#15673 = CARTESIAN_POINT ( 'NONE',  ( 1.411581201560190495E-15, 4.862606272033091592, -3.745885042887436622 ) ) ;
#15674 = AXIS2_PLACEMENT_3D ( 'NONE', #1788, #7706, #13906 ) ;
#15675 = FACE_OUTER_BOUND ( 'NONE', #14388, .T. ) ;
#15676 = CARTESIAN_POINT ( 'NONE',  ( -0.5711823568785978633, -5.381735091635035495, 0.6874999999999977796 ) ) ;
#15677 = CARTESIAN_POINT ( 'NONE',  ( -115.0000000000000142, -3.122502256758252770E-14, 17.50000000000000000 ) ) ;
#15678 = DIRECTION ( 'NONE',  ( 0.000000000000000000, 0.000000000000000000, 1.000000000000000000 ) ) ;
#15679 = CARTESIAN_POINT ( 'NONE',  ( -4.458734125000001214, -28.87500000136559564, 1.846868145590734089 ) ) ;
#15680 = ORIENTED_EDGE ( 'NONE', *, *, #3581, .F. ) ;
#15681 = CARTESIAN_POINT ( 'NONE',  ( 4.458734124999997661, -21.50000000136559208, 1.846868145590737864 ) ) ;
#15682 = DIRECTION ( 'NONE',  ( 0.000000000000000000, 1.000000000000000000, 0.000000000000000000 ) ) ;
#15683 = VERTEX_POINT ( 'NONE', #4898 ) ;
#15684 = AXIS2_PLACEMENT_3D ( 'NONE', #3179, #3108, #4397 ) ;
#15685 = VERTEX_POINT ( 'NONE', #12314 ) ;
#15686 = CARTESIAN_POINT ( 'NONE',  ( 5.000000000000000888, 0.000000000000000000, -9.999999999999998224 ) ) ;
#15687 = CARTESIAN_POINT ( 'NONE',  ( 4.458734125000000326, -28.37500000136559564, -1.846868145590734978 ) ) ;
#15688 = DIRECTION ( 'NONE',  ( 0.000000000000000000, -1.000000000000000000, 0.000000000000000000 ) ) ;
#15689 = ORIENTED_EDGE ( 'NONE', *, *, #1114, .F. ) ;
#15690 = LINE ( 'NONE', #8030, #15388 ) ;
#15691 = EDGE_CURVE ( 'NONE', #13261, #14412, #54, .T. ) ;
#15692 = EDGE_CURVE ( 'NONE', #2379, #5996, #7378, .T. ) ;
#15694 = AXIS2_PLACEMENT_3D ( 'NONE', #14143, #573, #14380 ) ;
#15693 = DIRECTION ( 'NONE',  ( -0.000000000000000000, 1.000000000000000000, -0.000000000000000000 ) ) ;
#15695 = AXIS2_PLACEMENT_3D ( 'NONE', #14356, #3285, #8232 ) ;
#15696 = CARTESIAN_POINT ( 'NONE',  ( -4.024497503033519941, -2.323544716729390558, -3.572167766733381544 ) ) ;
#15697 = CARTESIAN_POINT ( 'NONE',  ( -1.846868145590737420, -24.00000000136559564, 4.458734124999999437 ) ) ;
#15698 = DIRECTION ( 'NONE',  ( 1.000000000000000000, 0.000000000000000000, 1.114413700119375779E-16 ) ) ;
#15699 = CARTESIAN_POINT ( 'NONE',  ( 21.91530404932168352, -5.000000000000000000, -6.041579923254880136 ) ) ;
#15700 =( LENGTH_UNIT ( ) NAMED_UNIT ( * ) SI_UNIT ( .MILLI., .METRE. ) );
#15701 = AXIS2_PLACEMENT_3D ( 'NONE', #6513, #1500, #6439 ) ;
#15702 = CARTESIAN_POINT ( 'NONE',  ( -90.00000000000000000, -35.00000000000000711, -7.500000000000000000 ) ) ;
#15703 = ORIENTED_EDGE ( 'NONE', *, *, #11477, .F. ) ;
#15704 = VECTOR ( 'NONE', #15503, 1000.000000000000000 ) ;
#15705 = EDGE_LOOP ( 'NONE', ( #5712, #5055 ) ) ;
#15706 = CARTESIAN_POINT ( 'NONE',  ( -2.352174619735676320, 7.302225387958832137, -7.450218641349214188 ) ) ;
#15707 = AXIS2_PLACEMENT_3D ( 'NONE', #1229, #6011, #3823 ) ;
#15708 = VERTEX_POINT ( 'NONE', #6112 ) ;
#15709 =( REPRESENTATION_RELATIONSHIP ('NONE','NONE', #4176, #9778 ) REPRESENTATION_RELATIONSHIP_WITH_TRANSFORMATION ( #4213 )SHAPE_REPRESENTATION_RELATIONSHIP( ) );
#15710 = EDGE_CURVE ( 'NONE', #5167, #2220, #10254, .T. ) ;
#15711 = CIRCLE ( 'NONE', #1511, 4.000000000000000000 ) ;
#15712 = EDGE_CURVE ( 'NONE', #7839, #7795, #1251, .T. ) ;
#15713 = CARTESIAN_POINT ( 'NONE',  ( -5.000000000000000000, -26.50000000000000355, -6.123233995736766282E-16 ) ) ;
#15714 = CARTESIAN_POINT ( 'NONE',  ( 1.144235203016666258, 3.958177651039090250, -0.09382832055445661235 ) ) ;
#15715 = CARTESIAN_POINT ( 'NONE',  ( -4.276409079477644148, -1.261996585732578335, -0.8124999986344055847 ) ) ;
#15716 = AXIS2_PLACEMENT_3D ( 'NONE', #10798, #10946, #7247 ) ;
#15717 = DIRECTION ( 'NONE',  ( 1.000000000000000000, -6.123233995736766036E-17, -6.123233995736764803E-17 ) ) ;
#15718 = VECTOR ( 'NONE', #8838, 1000.000000000000000 ) ;
#15719 = PRODUCT_DEFINITION_SHAPE ( 'NONE', 'NONE',  #15970 ) ;
#15720 = CARTESIAN_POINT ( 'NONE',  ( -0.5093500532425060401, -4.799145180956616130, -1.874999998634406584 ) ) ;
#15721 = CARTESIAN_POINT ( 'NONE',  ( 0.000000000000000000, 0.000000000000000000, -25.03750572909317285 ) ) ;
#15722 = CARTESIAN_POINT ( 'NONE',  ( 3.535533905932738197, -22.00000000273118772, -3.535533905932738197 ) ) ;
#15723 = MECHANICAL_DESIGN_GEOMETRIC_PRESENTATION_REPRESENTATION (  '', ( #12861 ), #4088 ) ;
#15724 = ORIENTED_EDGE ( 'NONE', *, *, #5825, .F. ) ;
#15725 = CARTESIAN_POINT ( 'NONE',  ( 2.500000000000000000, 2.357898499370433054, -1.951563910473907981E-15 ) ) ;
#15726 = AXIS2_PLACEMENT_3D ( 'NONE', #8521, #1220, #12127 ) ;
#15727 = LINE ( 'NONE', #14341, #12759 ) ;
#15728 = ORIENTED_EDGE ( 'NONE', *, *, #991, .F. ) ;
#15729 = PLANE ( 'NONE',  #10832 ) ;
#15730 = ORIENTED_EDGE ( 'NONE', *, *, #7624, .T. ) ;
#15731 = ORIENTED_EDGE ( 'NONE', *, *, #11368, .F. ) ;
#15732 = EDGE_CURVE ( 'NONE', #6357, #10561, #9897, .T. ) ;
#15733 = AXIS2_PLACEMENT_3D ( 'NONE', #14052, #12830, #3308 ) ;
#15734 = EDGE_CURVE ( 'NONE', #15272, #8519, #1701, .T. ) ;
#15735 = VECTOR ( 'NONE', #406, 1000.000000000000000 ) ;
#15736 = EDGE_CURVE ( 'NONE', #6755, #14037, #7744, .T. ) ;
#15737 = LINE ( 'NONE', #11979, #14317 ) ;
#15738 = CARTESIAN_POINT ( 'NONE',  ( 30.02221399786052913, 88.59290746114278647, 16.00000000000001066 ) ) ;
#15739 = LINE ( 'NONE', #1013, #12677 ) ;
#15740 = DIRECTION ( 'NONE',  ( 0.000000000000000000, 0.000000000000000000, 1.000000000000000000 ) ) ;
#15741 = DIRECTION ( 'NONE',  ( 0.000000000000000000, 0.000000000000000000, -1.000000000000000000 ) ) ;
#15742 = CARTESIAN_POINT ( 'NONE',  ( 4.458734124999997661, -29.75000000136559564, 1.846868145590737864 ) ) ;
#15743 = CARTESIAN_POINT ( 'NONE',  ( 3.033343224707661712, -3.753672977998669946, 1.500000001365594304 ) ) ;
#15744 = ORIENTED_EDGE ( 'NONE', *, *, #8305, .T. ) ;
#15745 = AXIS2_PLACEMENT_3D ( 'NONE', #8372, #2122, #3418 ) ;
#15746 = DIRECTION ( 'NONE',  ( 0.000000000000000000, 0.000000000000000000, -1.000000000000000000 ) ) ;
#15747 = VERTEX_POINT ( 'NONE', #4326 ) ;
#15748 = ORIENTED_EDGE ( 'NONE', *, *, #3180, .F. ) ;
#15749 =( NAMED_UNIT ( * ) SI_UNIT ( $, .STERADIAN. ) SOLID_ANGLE_UNIT ( ) );
#15750 = ORIENTED_EDGE ( 'NONE', *, *, #9855, .T. ) ;
#15751 = CARTESIAN_POINT ( 'NONE',  ( 1.846868145590735200, -28.50000000136559564, -4.458734125000000326 ) ) ;
#15752 = DIRECTION ( 'NONE',  ( -1.000000000000000000, 0.000000000000000000, 0.000000000000000000 ) ) ;
#15753 = EDGE_CURVE ( 'NONE', #3455, #2036, #7494, .T. ) ;
#15754 = DIRECTION ( 'NONE',  ( 0.000000000000000000, 0.000000000000000000, 1.000000000000000000 ) ) ;
#15755 = CARTESIAN_POINT ( 'NONE',  ( -28.86751345948126257, -4.999999999999997335, -50.00000000000000711 ) ) ;
#15756 = PLANE ( 'NONE',  #1866 ) ;
#15757 =( BOUNDED_CURVE ( )  B_SPLINE_CURVE ( 2, ( #14985, #11339, #5200, #5363, #15060, #8926, #6498, #13835, #15140, #4058, #2844 ),
 .UNSPECIFIED., .F., .F. ) 
 B_SPLINE_CURVE_WITH_KNOTS ( ( 3, 2, 2, 2, 2, 3 ),
 ( 0.9045872658012773515, 0.9124999999999999778, 0.9250000000000000444, 0.9375000000000000000, 0.9499999999999999556, 0.9545872658012772849 ),
 .UNSPECIFIED. ) 
 CURVE ( )  GEOMETRIC_REPRESENTATION_ITEM ( )  RATIONAL_B_SPLINE_CURVE ( ( 0.9646335149384803742, 0.9518143178943441196, 1.000000000000000000, 0.9238795325112867385, 1.000000000000000000, 0.9238795325112867385, 1.000000000000000000, 0.9238795325112867385, 1.000000000000000000, 0.9720652146169428409, 0.9646335149384808183 ) ) 
 REPRESENTATION_ITEM ( '' )  );
#15758 = CARTESIAN_POINT ( 'NONE',  ( 0.000000000000000000, 0.000000000000000000, -25.03750572909317285 ) ) ;
#15759 = CARTESIAN_POINT ( 'NONE',  ( 4.795541693661363958, 1.415196051561583790, -3.000000000000002665 ) ) ;
#15760 = CARTESIAN_POINT ( 'NONE',  ( -3.535533905932738641, -21.50000000273118772, 3.535533905932737309 ) ) ;
#15761 = CARTESIAN_POINT ( 'NONE',  ( 1.797450215652874217, -4.579636122706331136, -0.06122359487011186374 ) ) ;
#15762 = CARTESIAN_POINT ( 'NONE',  ( 2.730187237215162345E-16, -31.18750000136559564, -4.458734124999999437 ) ) ;
#15763 = ORIENTED_EDGE ( 'NONE', *, *, #14503, .F. ) ;
#15764 = EDGE_CURVE ( 'NONE', #1547, #2790, #5215, .T. ) ;
#15765 = DIRECTION ( 'NONE',  ( 0.000000000000000000, 1.000000000000000000, 0.000000000000000000 ) ) ;
#15766 = ORIENTED_EDGE ( 'NONE', *, *, #9442, .F. ) ;
#15767 = ORIENTED_EDGE ( 'NONE', *, *, #1057, .F. ) ;
#15768 = CARTESIAN_POINT ( 'NONE',  ( -10.39117206796836079, 0.000000000000000000, -8.499999999999996447 ) ) ;
#15769 = CARTESIAN_POINT ( 'NONE',  ( 1.846868145590735200, -29.25000000136559564, -4.458734125000000326 ) ) ;
#15770 = DIRECTION ( 'NONE',  ( 0.5000000000000003331, 0.000000000000000000, -0.8660254037844385966 ) ) ;
#15771 = ORIENTED_EDGE ( 'NONE', *, *, #12775, .T. ) ;
#15772 = DIRECTION ( 'NONE',  ( 0.5000000000000002220, 0.000000000000000000, -0.8660254037844384856 ) ) ;
#15773 = CARTESIAN_POINT ( 'NONE',  ( -35.00000000000000000, 37.00000000000000000, -5.999999999999991118 ) ) ;
#15774 = DIRECTION ( 'NONE',  ( 1.000000000000000000, 0.000000000000000000, 0.000000000000000000 ) ) ;
#15775 = CARTESIAN_POINT ( 'NONE',  ( 39.69198092811959810, -4.097106062772730262, -28.32752661776758529 ) ) ;
#15776 = CARTESIAN_POINT ( 'NONE',  ( -4.458734124999999437, -23.18750000136559564, -5.460374474430324690E-16 ) ) ;
#15777 = CARTESIAN_POINT ( 'NONE',  ( 2.756197834950227410, 3.027510591568626896, -3.223146290109805356 ) ) ;
#15778 = CARTESIAN_POINT ( 'NONE',  ( 9.184850993605150311E-15, 37.00000000000000000, -75.00000000000001421 ) ) ;
#15779 = CARTESIAN_POINT ( 'NONE',  ( 2.071067811865475505, -30.93750000273118772, -5.000000000000000888 ) ) ;
#15780 = DIRECTION ( 'NONE',  ( 0.000000000000000000, 1.000000000000000000, 0.000000000000000000 ) ) ;
#15781 = EDGE_CURVE ( 'NONE', #15211, #2616, #10623, .T. ) ;
#15783 = EDGE_CURVE ( 'NONE', #8001, #13690, #11662, .T. ) ;
#15782 = ORIENTED_EDGE ( 'NONE', *, *, #11650, .F. ) ;
#15784 = VERTEX_POINT ( 'NONE', #13856 ) ;
#15785 = CARTESIAN_POINT ( 'NONE',  ( -90.00000000000000000, -35.00000000000000711, 7.500000000000001776 ) ) ;
#15786 = EDGE_LOOP ( 'NONE', ( #1653, #7726, #7435, #1800 ) ) ;
#15787 = FACE_OUTER_BOUND ( 'NONE', #14483, .T. ) ;
#15788 = LINE ( 'NONE', #4703, #2028 ) ;
#15789 = CARTESIAN_POINT ( 'NONE',  ( 3.916244202832140253, -2.131511515620588160, -1.437499998634406140 ) ) ;
#15790 = CARTESIAN_POINT ( 'NONE',  ( 1.918998964294743374E-15, 55.00000000000000711, -67.50000000000000000 ) ) ;
#15791 = CARTESIAN_POINT ( 'NONE',  ( 3.916244202832140253, -2.131511515620588160, -0.6874999986344089153 ) ) ;
#15792 = DIRECTION ( 'NONE',  ( -1.000000000000000000, 0.000000000000000000, 0.000000000000000000 ) ) ;
#15793 =( NAMED_UNIT ( * ) PLANE_ANGLE_UNIT ( ) SI_UNIT ( $, .RADIAN. ) );
#15794 = EDGE_CURVE ( 'NONE', #12316, #15603, #7924, .T. ) ;
#15795 = VERTEX_POINT ( 'NONE', #10321 ) ;
#15796 = CARTESIAN_POINT ( 'NONE',  ( 0.000000000000000000, 40.00000000000000000, 0.000000000000000000 ) ) ;
#15797 = PRODUCT_DEFINITION ( 'UNKNOWN', '', #12039, #7563 ) ;
#15798 =( REPRESENTATION_RELATIONSHIP ('NONE','NONE', #4176, #4696 ) REPRESENTATION_RELATIONSHIP_WITH_TRANSFORMATION ( #13673 )SHAPE_REPRESENTATION_RELATIONSHIP( ) );
#15799 =( LENGTH_UNIT ( ) NAMED_UNIT ( * ) SI_UNIT ( .MILLI., .METRE. ) );
#15800 = ORIENTED_EDGE ( 'NONE', *, *, #4108, .F. ) ;
#15801 = DIRECTION ( 'NONE',  ( 0.000000000000000000, 0.000000000000000000, -1.000000000000000000 ) ) ;
#15802 = ORIENTED_EDGE ( 'NONE', *, *, #14475, .F. ) ;
#15803 = ORIENTED_EDGE ( 'NONE', *, *, #1953, .F. ) ;
#15804 = CARTESIAN_POINT ( 'NONE',  ( 1.261996585732578113, -4.276409079477644148, -1.812499998634406584 ) ) ;
#15805 = VECTOR ( 'NONE', #2757, 1000.000000000000000 ) ;
#15806 = DIRECTION ( 'NONE',  ( 0.000000000000000000, 1.000000000000000000, 0.000000000000000000 ) ) ;
#15807 = DIRECTION ( 'NONE',  ( 0.000000000000000000, 1.000000000000000000, 0.000000000000000000 ) ) ;
#15808 = DIRECTION ( 'NONE',  ( 0.000000000000000000, 0.000000000000000000, 1.000000000000000000 ) ) ;
#15809 = CARTESIAN_POINT ( 'NONE',  ( -5.000000000000000000, -29.62500000273118417, -6.123233995736766282E-16 ) ) ;
#15810 = CARTESIAN_POINT ( 'NONE',  ( -4.209348295687703967, -3.401574460001763001, -0.3124999972688167760 ) ) ;
#15811 = CARTESIAN_POINT ( 'NONE',  ( -21.01110699893060030, -3.000000000000001332, 36.39230484541324273 ) ) ;
#15812 = ADVANCED_FACE ( 'NONE', ( #13767, #2701, #4156 ), #15247, .F. ) ;
#15813 = CARTESIAN_POINT ( 'NONE',  ( 3.152801135295366208, -24.81250000136559564, 3.152801135295367985 ) ) ;
#15814 = EDGE_CURVE ( 'NONE', #9703, #14592, #8406, .T. ) ;
#15815 = EDGE_CURVE ( 'NONE', #15506, #12880, #1503, .T. ) ;
#15816 = CARTESIAN_POINT ( 'NONE',  ( -3.033343224707664376, 3.753672977998667726, -3.999999998634406140 ) ) ;
#15817 = VERTEX_POINT ( 'NONE', #10151 ) ;
#15818 = CARTESIAN_POINT ( 'NONE',  ( 35.00000000000000000, 50.00000000000000000, 0.000000000000000000 ) ) ;
#15819 = VERTEX_POINT ( 'NONE', #305 ) ;
#15820 = ORIENTED_EDGE ( 'NONE', *, *, #11333, .F. ) ;
#15821 = VERTEX_POINT ( 'NONE', #15074 ) ;
#15822 = CARTESIAN_POINT ( 'NONE',  ( 14.41154273188008439, 0.000000000000000000, 60.96152422706632024 ) ) ;
#15823 = DIRECTION ( 'NONE',  ( -0.000000000000000000, -1.000000000000000000, -0.000000000000000000 ) ) ;
#15824 = DIRECTION ( 'NONE',  ( -1.000000000000000000, -1.982541115402065110E-16, 0.000000000000000000 ) ) ;
#15825 = VECTOR ( 'NONE', #8505, 1000.000000000000000 ) ;
#15826 = DIRECTION ( 'NONE',  ( 0.000000000000000000, 0.000000000000000000, 1.000000000000000000 ) ) ;
#15827 = CARTESIAN_POINT ( 'NONE',  ( 4.841222716689082439, -4.462727778340696005, 48.49605756500809406 ) ) ;
#15828 = LINE ( 'NONE', #4748, #6434 ) ;
#15829 = CARTESIAN_POINT ( 'NONE',  ( 4.795541693661363958, 1.415196051561583790, -1.000000000000000888 ) ) ;
#15830 = DIRECTION ( 'NONE',  ( -1.000000000000000000, -0.000000000000000000, -0.000000000000000000 ) ) ;
#15831 = CARTESIAN_POINT ( 'NONE',  ( -5.000000000000000000, -27.50000000000000000, -6.123233995736766282E-16 ) ) ;
#15832 = CARTESIAN_POINT ( 'NONE',  ( -4.458734125000001214, -30.87500000136559564, 1.846868145590734089 ) ) ;
#15833 = EDGE_CURVE ( 'NONE', #2885, #7703, #6580, .T. ) ;
#15834 = ADVANCED_BREP_SHAPE_REPRESENTATION ( '', ( #9140, #3223 ), #7084 ) ;
#15835 = CARTESIAN_POINT ( 'NONE',  ( 1.261996585732578113, -4.276409079477644148, -0.8124999986344090264 ) ) ;
#15836 = ORIENTED_EDGE ( 'NONE', *, *, #1439, .F. ) ;
#15837 = CARTESIAN_POINT ( 'NONE',  ( -19.99999999999956657, -13.00000000000000178, 8.786575603324269439E-13 ) ) ;
#15838 = VERTEX_POINT ( 'NONE', #542 ) ;
#15839 = EDGE_LOOP ( 'NONE', ( #3703, #10846, #323, #12935 ) ) ;
#15840 = DIRECTION ( 'NONE',  ( -0.7071067811865306973, 0.000000000000000000, 0.7071067811865643371 ) ) ;
#15841 = CARTESIAN_POINT ( 'NONE',  ( 1.846868145590735200, -28.25000000136559208, -4.458734125000000326 ) ) ;
#15842 = DIRECTION ( 'NONE',  ( 0.000000000000000000, 0.000000000000000000, 1.000000000000000000 ) ) ;
#15843 = EDGE_LOOP ( 'NONE', ( #15062, #2581, #11531, #8333 ) ) ;
#15844 = DIRECTION ( 'NONE',  ( -0.005931855436079598413, 0.9999824063907751803, 0.000000000000000000 ) ) ;
#15845 =( BOUNDED_CURVE ( )  B_SPLINE_CURVE ( 2, ( #10997, #3881, #7530, #7216, #12118, #1054, #14636, #12272, #6235, #1128, #6068 ),
 .UNSPECIFIED., .F., .F. ) 
 B_SPLINE_CURVE_WITH_KNOTS ( ( 3, 2, 2, 2, 2, 3 ),
 ( 0.7045872658012772849, 0.7125000000000000222, 0.7249999999999999778, 0.7375000000000000444, 0.7500000000000000000, 0.7545872658012773293 ),
 .UNSPECIFIED. ) 
 CURVE ( )  GEOMETRIC_REPRESENTATION_ITEM ( )  RATIONAL_B_SPLINE_CURVE ( ( 0.9646335149384808183, 0.9518143178943441196, 1.000000000000000000, 0.9238795325112867385, 1.000000000000000000, 0.9238795325112867385, 1.000000000000000000, 0.9238795325112867385, 1.000000000000000000, 0.9720652146169423968, 0.9646335149384803742 ) ) 
 REPRESENTATION_ITEM ( '' )  );
#15846 = PRODUCT_DEFINITION_SHAPE ( 'NONE', 'NONE',  #6026 ) ;
#15847 = DIRECTION ( 'NONE',  ( 0.000000000000000000, -1.000000000000000000, 0.000000000000000000 ) ) ;
#15848 = FACE_OUTER_BOUND ( 'NONE', #5771, .T. ) ;
#15849 = DIRECTION ( 'NONE',  ( 0.000000000000000000, 0.000000000000000000, 1.000000000000000000 ) ) ;
#15850 = CARTESIAN_POINT ( 'NONE',  ( -4.458734125000001214, -22.12500000136559564, 1.846868145590734089 ) ) ;
#15851 = LINE ( 'NONE', #10026, #6835 ) ;
#15852 = CARTESIAN_POINT ( 'NONE',  ( -4.795541693661363958, -1.415196051561583790, -1.374999997268814500 ) ) ;
#15853 = CARTESIAN_POINT ( 'NONE',  ( 5.274401269815137461, 6.074457022762082659, -7.633824513837106807 ) ) ;
#15854 = LINE ( 'NONE', #3555, #7702 ) ;
#15855 = DIRECTION ( 'NONE',  ( 0.000000000000000000, -1.000000000000000000, 0.000000000000000000 ) ) ;
#15856 = ORIENTED_EDGE ( 'NONE', *, *, #10134, .F. ) ;
#15857 = FILL_AREA_STYLE_COLOUR ( '', #7610 ) ;
#15858 = ORIENTED_EDGE ( 'NONE', *, *, #6006, .T. ) ;
#15859 = CYLINDRICAL_SURFACE ( 'NONE', #12518, 29.99999999999999289 ) ;
#15860 = ORIENTED_EDGE ( 'NONE', *, *, #10086, .T. ) ;
#15861 = CARTESIAN_POINT ( 'NONE',  ( 17.00000000000000000, 0.000000000000000000, 0.000000000000000000 ) ) ;
#15862 = ADVANCED_FACE ( 'NONE', ( #2787 ), #13268, .F. ) ;
#15863 = AXIS2_PLACEMENT_3D ( 'NONE', #6780, #9364, #8251 ) ;
#15864 = TOROIDAL_SURFACE ( 'NONE', #2173, 10.12668159690567649, 0.7733184030943209830 ) ;
#15865 = CARTESIAN_POINT ( 'NONE',  ( 5.000000000000004441, -2.247904837838113790E-16, -3.920263044861760360 ) ) ;
#15866 = CARTESIAN_POINT ( 'NONE',  ( 3.535533905932736864, -28.12500000000000000, 3.535533905932738641 ) ) ;
#15867 = CARTESIAN_POINT ( 'NONE',  ( -21.01110699893060030, -7.999999999999996447, 36.39230484541324273 ) ) ;
#15868 = CARTESIAN_POINT ( 'NONE',  ( 4.799145180956616130, -0.5093500532425063732, -2.624999998634407028 ) ) ;
#15869 = FACE_OUTER_BOUND ( 'NONE', #9052, .T. ) ;
#15870 = CARTESIAN_POINT ( 'NONE',  ( 5.000000000000000888, -22.06250000273118772, -2.071067811865475505 ) ) ;
#15871 = VERTEX_POINT ( 'NONE', #10389 ) ;
#15872 = DIRECTION ( 'NONE',  ( -1.000000000000000000, 0.000000000000000000, 0.000000000000000000 ) ) ;
#15873 = AXIS2_PLACEMENT_3D ( 'NONE', #10122, #1381, #13825 ) ;
#15874 = ORIENTED_EDGE ( 'NONE', *, *, #5435, .F. ) ;
#15875 = CARTESIAN_POINT ( 'NONE',  ( 4.000000000000000888, -0.8578082829538523635, -3.433262215449808696 ) ) ;
#15876 = CYLINDRICAL_SURFACE ( 'NONE', #6100, 2.649999999999992806 ) ;
#15877 = AXIS2_PLACEMENT_3D ( 'NONE', #4722, #10792, #8458 ) ;
#15878 = VERTEX_POINT ( 'NONE', #12711 ) ;
#15879 = CARTESIAN_POINT ( 'NONE',  ( -3.753672977998669502, -3.033343224707661712, -4.999999998634407028 ) ) ;
#15880 = CARTESIAN_POINT ( 'NONE',  ( -67.50000000000000000, 50.00000000000000000, -2.650000000000692690 ) ) ;
#15881 = ADVANCED_FACE ( 'NONE', ( #6515 ), #10235, .T. ) ;
#15882 = EDGE_CURVE ( 'NONE', #5376, #11530, #845, .T. ) ;
#15883 = VECTOR ( 'NONE', #5399, 1000.000000000000000 ) ;
#15884 = CARTESIAN_POINT ( 'NONE',  ( 21.99999999999956657, -8.786575603324269439E-13, 0.000000000000000000 ) ) ;
#15885 = CARTESIAN_POINT ( 'NONE',  ( 2.500000000000000000, -2.357898499370432610, 3.252606517456513302E-15 ) ) ;
#15886 = CARTESIAN_POINT ( 'NONE',  ( -0.5711823568785977523, -5.381735091635034607, -2.312500000000001332 ) ) ;
#15887 = CIRCLE ( 'NONE', #8928, 5.999999999999991118 ) ;
#15888 = CARTESIAN_POINT ( 'NONE',  ( 2.500000000000000000, -1.768423874527823791, -1.020999999999998353 ) ) ;
#15889 = CARTESIAN_POINT ( 'NONE',  ( 1.605140903214875142E-15, -8.895730773063899477, -7.917997657324742811 ) ) ;
#15890 = CARTESIAN_POINT ( 'NONE',  ( 0.000000000000000000, -2.357898499370432610, 3.252606517456513302E-15 ) ) ;
#15891 = APPLICATION_CONTEXT ( 'automotive_design' ) ;
#15892 = SURFACE_STYLE_FILL_AREA ( #5868 ) ;
#15893 = CARTESIAN_POINT ( 'NONE',  ( 1.846868145590735200, -26.50000000136559564, -4.458734124999999437 ) ) ;
#15894 = CARTESIAN_POINT ( 'NONE',  ( 4.276409079477644148, 1.261996585732577891, -5.312499998634406140 ) ) ;
#15895 = DIRECTION ( 'NONE',  ( -1.000000000000000000, -0.000000000000000000, -0.000000000000000000 ) ) ;
#15896 = VERTEX_POINT ( 'NONE', #3349 ) ;
#15897 = EDGE_LOOP ( 'NONE', ( #13208, #13207, #2396, #8079 ) ) ;
#15899 = AXIS2_PLACEMENT_3D ( 'NONE', #266, #10110, #2493 ) ;
#15898 = FILL_AREA_STYLE ('',( #6034 ) ) ;
#15900 = ORIENTED_EDGE ( 'NONE', *, *, #10924, .T. ) ;
#15901 = CARTESIAN_POINT ( 'NONE',  ( 1.846868145590735200, -22.50000000136559208, -4.458734125000000326 ) ) ;
#15902 = DIRECTION ( 'NONE',  ( -0.000000000000000000, -1.000000000000000000, -0.000000000000000000 ) ) ;
#15903 = PLANE ( 'NONE',  #8648 ) ;
#15904 = EDGE_CURVE ( 'NONE', #8839, #7386, #8055, .T. ) ;
#15905 = EDGE_CURVE ( 'NONE', #1506, #4542, #15727, .T. ) ;
#15906 = DIRECTION ( 'NONE',  ( 0.8660254037844410391, -0.4999999999999960032, -1.895741069380448091E-15 ) ) ;
#15907 = CARTESIAN_POINT ( 'NONE',  ( 4.621606065640972538, -3.978804951770222420, 48.55546797644264245 ) ) ;
#15908 = DIRECTION ( 'NONE',  ( -1.000000000000000000, -0.000000000000000000, -0.000000000000000000 ) ) ;
#15909 = VECTOR ( 'NONE', #13607, 1000.000000000000000 ) ;
#15910 = CARTESIAN_POINT ( 'NONE',  ( -0.5711823568785978633, -5.381735091635035495, -3.312500000000001776 ) ) ;
#15911 = LINE ( 'NONE', #14694, #9879 ) ;
#15912 = DIRECTION ( 'NONE',  ( 1.000000000000000000, 0.000000000000000000, 0.000000000000000000 ) ) ;
#15913 = CARTESIAN_POINT ( 'NONE',  ( -3.152801135295367985, -26.81250000136559564, 3.152801135295367096 ) ) ;
#15914 = VECTOR ( 'NONE', #12495, 1000.000000000000000 ) ;
#15915 = CARTESIAN_POINT ( 'NONE',  ( -0.5093500532425060401, -4.799145180956616130, -0.8749999986344056957 ) ) ;
#15916 = ORIENTED_EDGE ( 'NONE', *, *, #5702, .T. ) ;
#15917 = CLOSED_SHELL ( 'NONE', ( #8953, #15293, #11160, #14623, #2030, #15575, #12639, #3364, #8978, #11529, #4230, #10380, #6937, #14716, #5781, #9743, #8240, #10828, #14311, #10488, #7375, #8180, #13400, #8290, #6029, #14783, #6325 ) ) ;
#15918 = CARTESIAN_POINT ( 'NONE',  ( 42.02221399786069611, -3.000000000000000000, 1.040834085586084257E-13 ) ) ;
#15919 = EDGE_LOOP ( 'NONE', ( #11663, #14517, #11689, #15803 ) ) ;
#15920 = VERTEX_POINT ( 'NONE', #10630 ) ;
#15921 = CYLINDRICAL_SURFACE ( 'NONE', #7995, 5.000000000000000000 ) ;
#15922 = CARTESIAN_POINT ( 'NONE',  ( 4.458734124999999437, -23.43750000136559564, 0.000000000000000000 ) ) ;
#15923 = CARTESIAN_POINT ( 'NONE',  ( 2.500000000000000000, 1.768423874527824902, 1.020999999999999019 ) ) ;
#15924 = EDGE_LOOP ( 'NONE', ( #6595, #10707, #9943, #13931 ) ) ;
#15925 = CARTESIAN_POINT ( 'NONE',  ( -2.886751345948103342, -37.00000000000000711, -35.00000000000000000 ) ) ;
#15926 = AXIS2_PLACEMENT_3D ( 'NONE', #3646, #6322, #11240 ) ;
#15927 = EDGE_CURVE ( 'NONE', #15685, #1580, #2053, .T. ) ;
#15928 = DIRECTION ( 'NONE',  ( 0.000000000000000000, 1.000000000000000000, 0.000000000000000000 ) ) ;
#15929 = CARTESIAN_POINT ( 'NONE',  ( 0.000000000000000000, 0.000000000000000000, 0.000000000000000000 ) ) ;
#15930 = DIRECTION ( 'NONE',  ( -1.000000000000000000, 0.000000000000000000, 0.000000000000000000 ) ) ;
#15931 = CARTESIAN_POINT ( 'NONE',  ( 4.458734124999999437, -22.75000000136559208, 1.846868145590737864 ) ) ;
#15932 = CARTESIAN_POINT ( 'NONE',  ( -99.99999999999998579, -35.00000000000000711, 17.50000000000000000 ) ) ;
#15933 = AXIS2_PLACEMENT_3D ( 'NONE', #9998, #1338, #8954 ) ;
#15934 = DIRECTION ( 'NONE',  ( 0.000000000000000000, 0.000000000000000000, -1.000000000000000000 ) ) ;
#15935 = CARTESIAN_POINT ( 'NONE',  ( -9.184850993605147944E-16, -27.37500000273118772, 5.000000000000000000 ) ) ;
#15936 = CARTESIAN_POINT ( 'NONE',  ( 7.500000000000003553, -4.330127018922199866, -7.422398894150035176 ) ) ;
#15937 = FACE_OUTER_BOUND ( 'NONE', #12138, .T. ) ;
#15938 = VERTEX_POINT ( 'NONE', #1003 ) ;
#15939 = AXIS2_PLACEMENT_3D ( 'NONE', #4879, #7385, #6178 ) ;
#15940 = SURFACE_STYLE_USAGE ( .BOTH. , #2268 ) ;
#15941 = ORIENTED_EDGE ( 'NONE', *, *, #3148, .F. ) ;
#15942 = DIRECTION ( 'NONE',  ( 1.000000000000000000, 0.000000000000000000, 0.000000000000000000 ) ) ;
#15943 =( BOUNDED_CURVE ( )  B_SPLINE_CURVE ( 2, ( #4411, #11902, #2126, #9420, #12957, #5699, #11746, #14195, #5772 ),
 .UNSPECIFIED., .F., .F. ) 
 B_SPLINE_CURVE_WITH_KNOTS ( ( 3, 2, 2, 2, 3 ),
 ( 0.7750000000000000222, 0.7874999999999999778, 0.8000000000000000444, 0.8125000000000001110, 0.8250000000000000666 ),
 .UNSPECIFIED. ) 
 CURVE ( )  GEOMETRIC_REPRESENTATION_ITEM ( )  RATIONAL_B_SPLINE_CURVE ( ( 1.000000000000000000, 0.9238795325112867385, 1.000000000000000000, 0.9238795325112867385, 1.000000000000000000, 0.9238795325112867385, 1.000000000000000000, 0.9238795325112860723, 1.000000000000000666 ) ) 
 REPRESENTATION_ITEM ( '' )  );
#15944 = EDGE_LOOP ( 'NONE', ( #13951, #4630, #10860, #10450, #8971 ) ) ;
#15945 = DIRECTION ( 'NONE',  ( 0.000000000000000000, 0.000000000000000000, 1.000000000000000000 ) ) ;
#15946 = AXIS2_PLACEMENT_3D ( 'NONE', #15501, #14276, #11838 ) ;
#15947 = ADVANCED_FACE ( 'NONE', ( #10704 ), #5767, .F. ) ;
#15948 = CARTESIAN_POINT ( 'NONE',  ( -5.000000000000000000, -25.62500000273118417, -6.123233995736766282E-16 ) ) ;
#15949 = CIRCLE ( 'NONE', #4064, 2.500000000000000444 ) ;
#15950 = CARTESIAN_POINT ( 'NONE',  ( 3.916244202832140253, -2.131511515620588160, 0.5625000013655921949 ) ) ;
#15951 = DIRECTION ( 'NONE',  ( 0.8660254037844432595, 0.000000000000000000, -0.4999999999999919509 ) ) ;
#15952 = CARTESIAN_POINT ( 'NONE',  ( -2.131511515620587272, -3.916244202832140253, -0.9374999986344056957 ) ) ;
#15953 = SURFACE_STYLE_FILL_AREA ( #14565 ) ;
#15954 = AXIS2_PLACEMENT_3D ( 'NONE', #12571, #8799, #7673 ) ;
#15955 = FACE_OUTER_BOUND ( 'NONE', #1190, .T. ) ;
#15956 = EDGE_CURVE ( 'NONE', #15563, #10113, #4558, .T. ) ;
#15957 = VERTEX_POINT ( 'NONE', #9414 ) ;
#15958 = PLANE ( 'NONE',  #5157 ) ;
#15959 = ORIENTED_EDGE ( 'NONE', *, *, #11636, .F. ) ;
#15960 = CIRCLE ( 'NONE', #5895, 2.649999999999992806 ) ;
#15961 = AXIS2_PLACEMENT_3D ( 'NONE', #11143, #13314, #1121 ) ;
#15962 = EDGE_LOOP ( 'NONE', ( #10978, #1473, #11961, #14450, #3658 ) ) ;
#15963 = CARTESIAN_POINT ( 'NONE',  ( -4.799145180956616130, 0.5093500532425063732, -1.124999998634405918 ) ) ;
#15964 = DIRECTION ( 'NONE',  ( -0.000000000000000000, 1.000000000000000000, -0.000000000000000000 ) ) ;
#15965 = ORIENTED_EDGE ( 'NONE', *, *, #3086, .F. ) ;
#15966 = NEXT_ASSEMBLY_USAGE_OCCURRENCE ( 'NAUO1', ' ', ' ', #5020, #4824, $ ) ;
#15967 = NEXT_ASSEMBLY_USAGE_OCCURRENCE ( 'NAUO2', ' ', ' ', #5020, #6009, $ ) ;
#15968 = NEXT_ASSEMBLY_USAGE_OCCURRENCE ( 'NAUO3', ' ', ' ', #5020, #11724, $ ) ;
#15969 = NEXT_ASSEMBLY_USAGE_OCCURRENCE ( 'NAUO4', ' ', ' ', #5020, #15797, $ ) ;
#15970 = NEXT_ASSEMBLY_USAGE_OCCURRENCE ( 'NAUO5', ' ', ' ', #5020, #2153, $ ) ;
#15971 = NEXT_ASSEMBLY_USAGE_OCCURRENCE ( 'NAUO6', ' ', ' ', #5020, #6723, $ ) ;
#15972 = NEXT_ASSEMBLY_USAGE_OCCURRENCE ( 'NAUO7', ' ', ' ', #5020, #6223, $ ) ;
#15973 = NEXT_ASSEMBLY_USAGE_OCCURRENCE ( 'NAUO8', ' ', ' ', #5020, #6723, $ ) ;
#15974 = NEXT_ASSEMBLY_USAGE_OCCURRENCE ( 'NAUO9', ' ', ' ', #5020, #6723, $ ) ;
#15975 = NEXT_ASSEMBLY_USAGE_OCCURRENCE ( 'NAUO10', ' ', ' ', #5020, #2153, $ ) ;
#15976 = NEXT_ASSEMBLY_USAGE_OCCURRENCE ( 'NAUO11', ' ', ' ', #5020, #2153, $ ) ;
#15977 = NEXT_ASSEMBLY_USAGE_OCCURRENCE ( 'NAUO12', ' ', ' ', #5020, #6026, $ ) ;
#15978 = NEXT_ASSEMBLY_USAGE_OCCURRENCE ( 'NAUO13', ' ', ' ', #5020, #13413, $ ) ;
#15979 = NEXT_ASSEMBLY_USAGE_OCCURRENCE ( 'NAUO14', ' ', ' ', #5020, #8905, $ ) ;
#15980 = NEXT_ASSEMBLY_USAGE_OCCURRENCE ( 'NAUO15', ' ', ' ', #5020, #8905, $ ) ;
#15981 = NEXT_ASSEMBLY_USAGE_OCCURRENCE ( 'NAUO16', ' ', ' ', #5020, #8905, $ ) ;
#15982 = NEXT_ASSEMBLY_USAGE_OCCURRENCE ( 'NAUO17', ' ', ' ', #5020, #13413, $ ) ;
#15983 = NEXT_ASSEMBLY_USAGE_OCCURRENCE ( 'NAUO18', ' ', ' ', #5020, #13413, $ ) ;
#15984 = NEXT_ASSEMBLY_USAGE_OCCURRENCE ( 'NAUO19', ' ', ' ', #5020, #501, $ ) ;
#15985 = NEXT_ASSEMBLY_USAGE_OCCURRENCE ( 'NAUO20', ' ', ' ', #5020, #501, $ ) ;
#15986 = NEXT_ASSEMBLY_USAGE_OCCURRENCE ( 'NAUO21', ' ', ' ', #5020, #501, $ ) ;
#15987 = NEXT_ASSEMBLY_USAGE_OCCURRENCE ( 'NAUO22', ' ', ' ', #5020, #1484, $ ) ;
#15988 = NEXT_ASSEMBLY_USAGE_OCCURRENCE ( 'NAUO23', ' ', ' ', #5020, #1484, $ ) ;
#15989 = NEXT_ASSEMBLY_USAGE_OCCURRENCE ( 'NAUO24', ' ', ' ', #5020, #1484, $ ) ;
#15990 = NEXT_ASSEMBLY_USAGE_OCCURRENCE ( 'NAUO25', ' ', ' ', #5020, #1484, $ ) ;
#15991 = NEXT_ASSEMBLY_USAGE_OCCURRENCE ( 'NAUO26', ' ', ' ', #5020, #12418, $ ) ;
#15992 = NEXT_ASSEMBLY_USAGE_OCCURRENCE ( 'NAUO27', ' ', ' ', #5020, #12418, $ ) ;
#15993 = NEXT_ASSEMBLY_USAGE_OCCURRENCE ( 'NAUO28', ' ', ' ', #5020, #12418, $ ) ;
#15994 = NEXT_ASSEMBLY_USAGE_OCCURRENCE ( 'NAUO29', ' ', ' ', #5020, #12418, $ ) ;
#15995 = NEXT_ASSEMBLY_USAGE_OCCURRENCE ( 'NAUO30', ' ', ' ', #5020, #12418, $ ) ;
#15996 = NEXT_ASSEMBLY_USAGE_OCCURRENCE ( 'NAUO31', ' ', ' ', #5020, #12418, $ ) ;
#15997 = NEXT_ASSEMBLY_USAGE_OCCURRENCE ( 'NAUO32', ' ', ' ', #5020, #12418, $ ) ;
#15998 = NEXT_ASSEMBLY_USAGE_OCCURRENCE ( 'NAUO33', ' ', ' ', #5020, #1484, $ ) ;
#15999 = NEXT_ASSEMBLY_USAGE_OCCURRENCE ( 'NAUO34', ' ', ' ', #5020, #1484, $ ) ;
#16000 = NEXT_ASSEMBLY_USAGE_OCCURRENCE ( 'NAUO35', ' ', ' ', #5020, #12418, $ ) ;
#16001 = NEXT_ASSEMBLY_USAGE_OCCURRENCE ( 'NAUO36', ' ', ' ', #5020, #12418, $ ) ;
ENDSEC;
END-ISO-10303-21;
